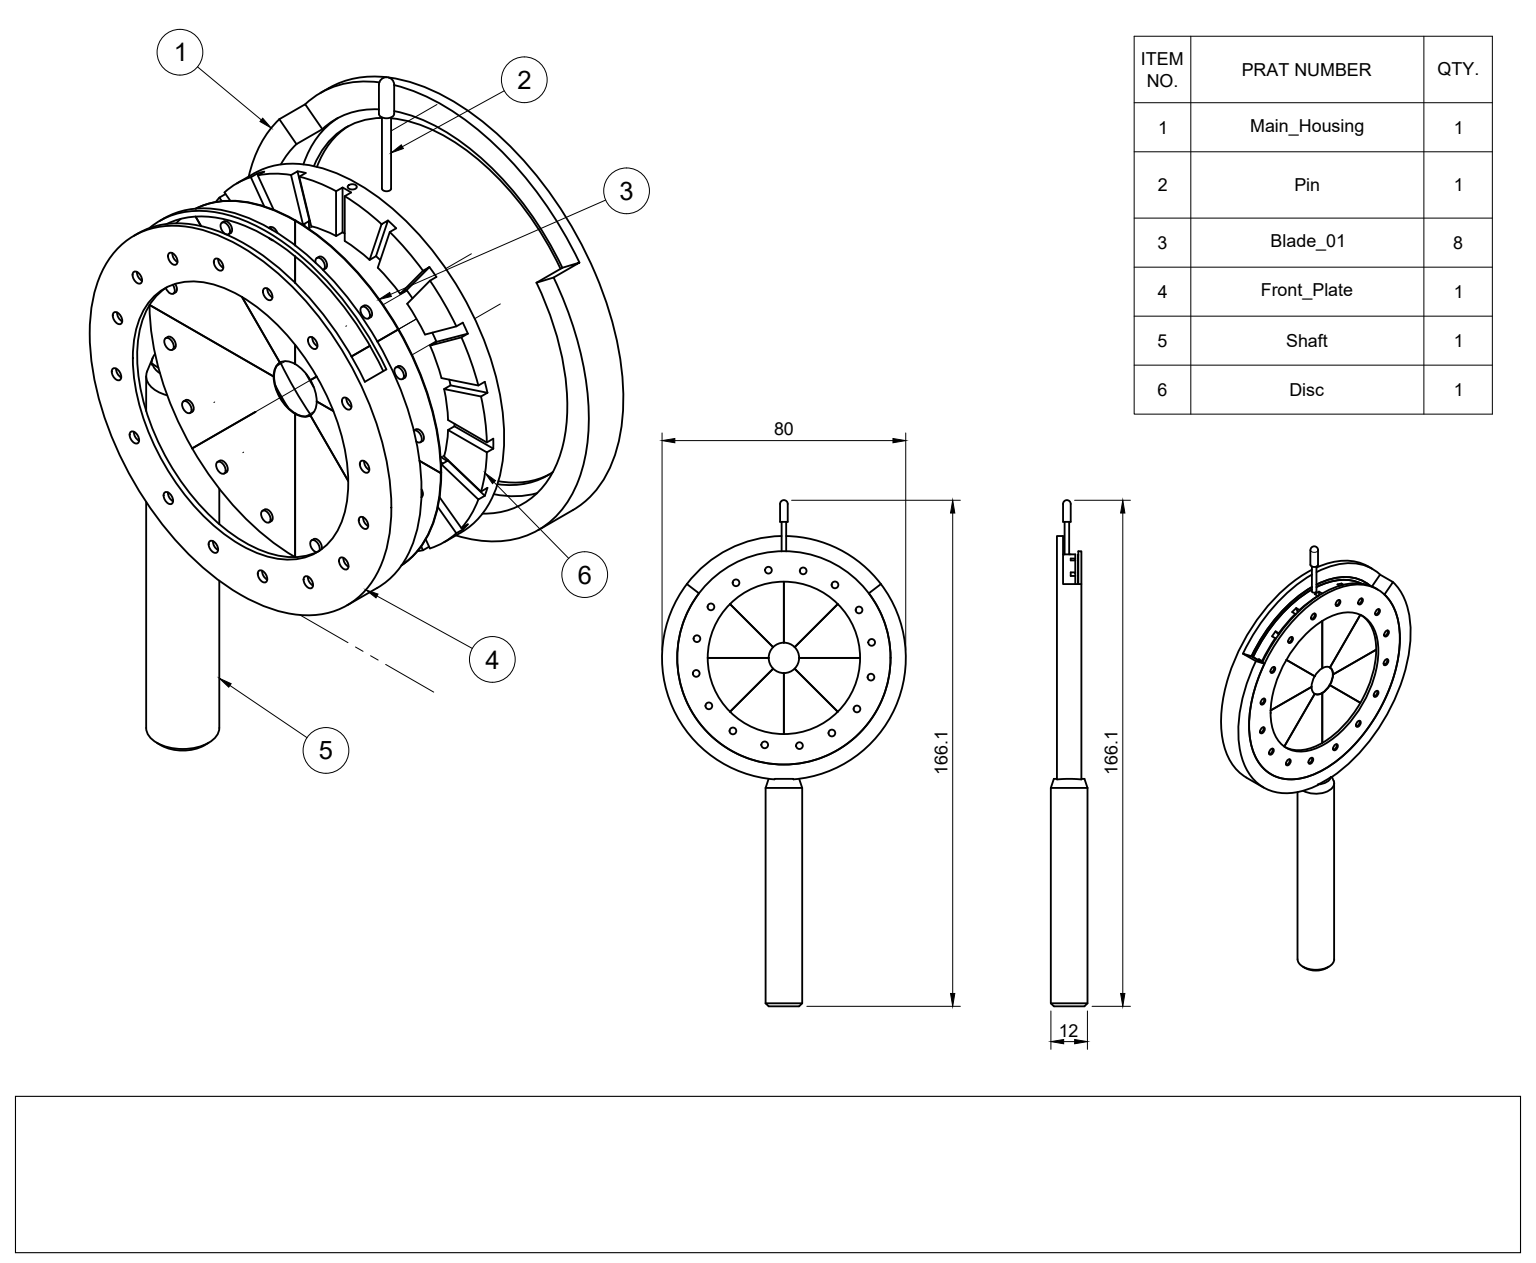
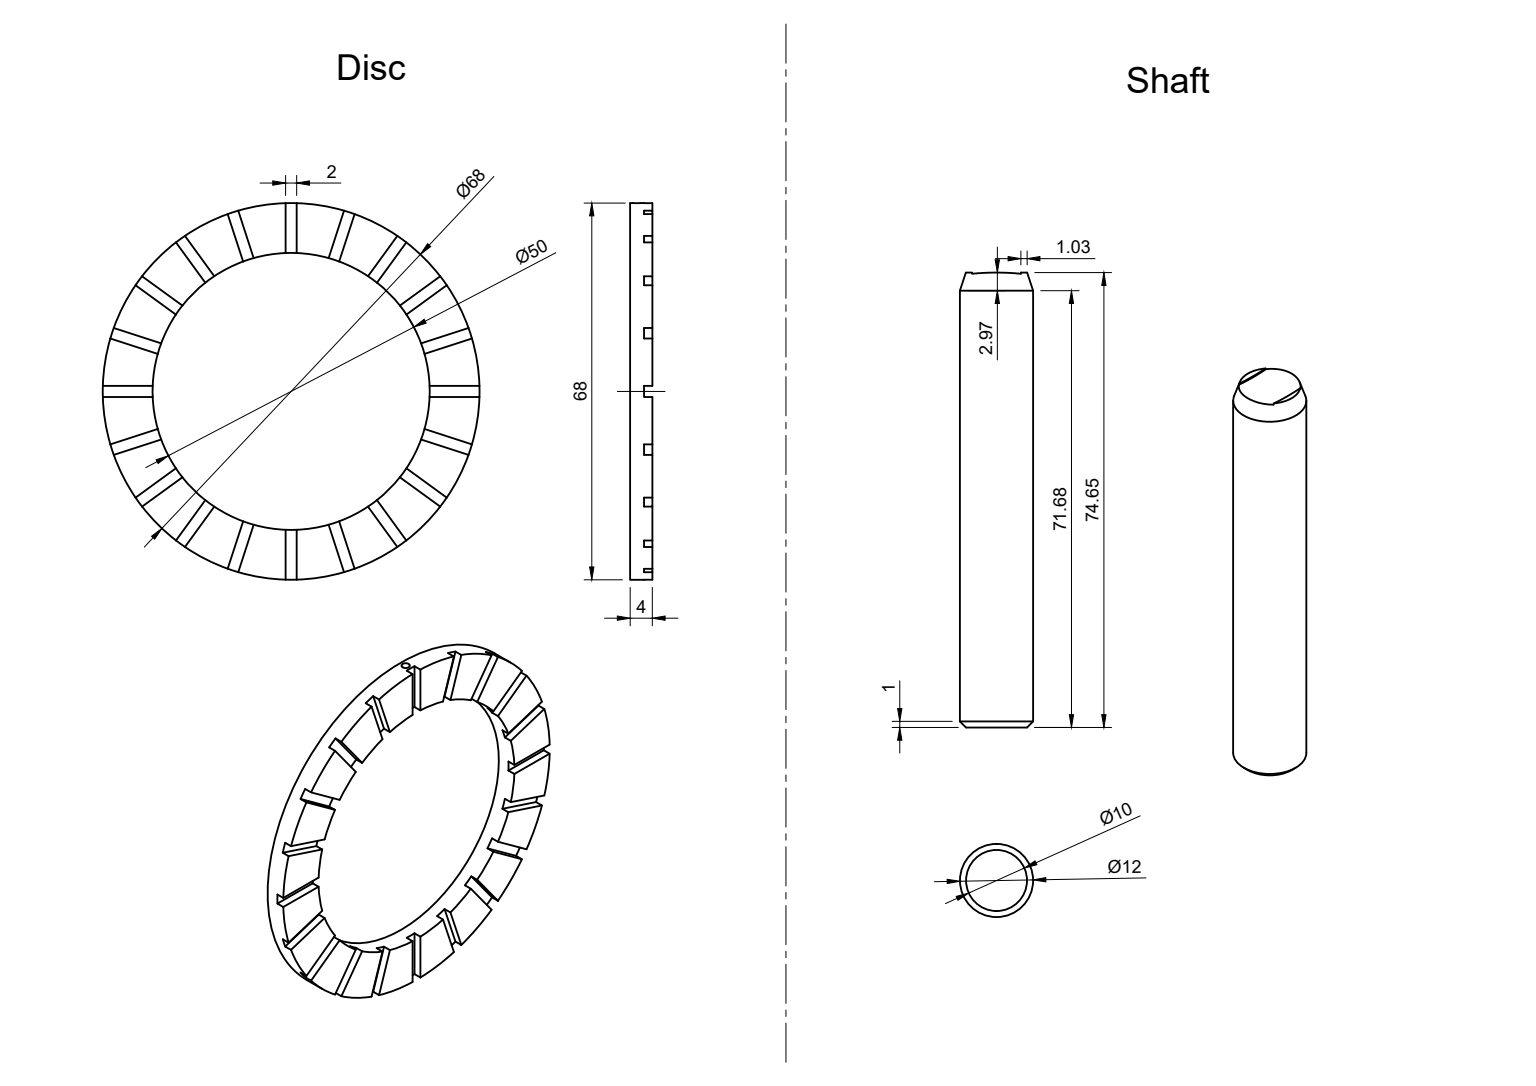
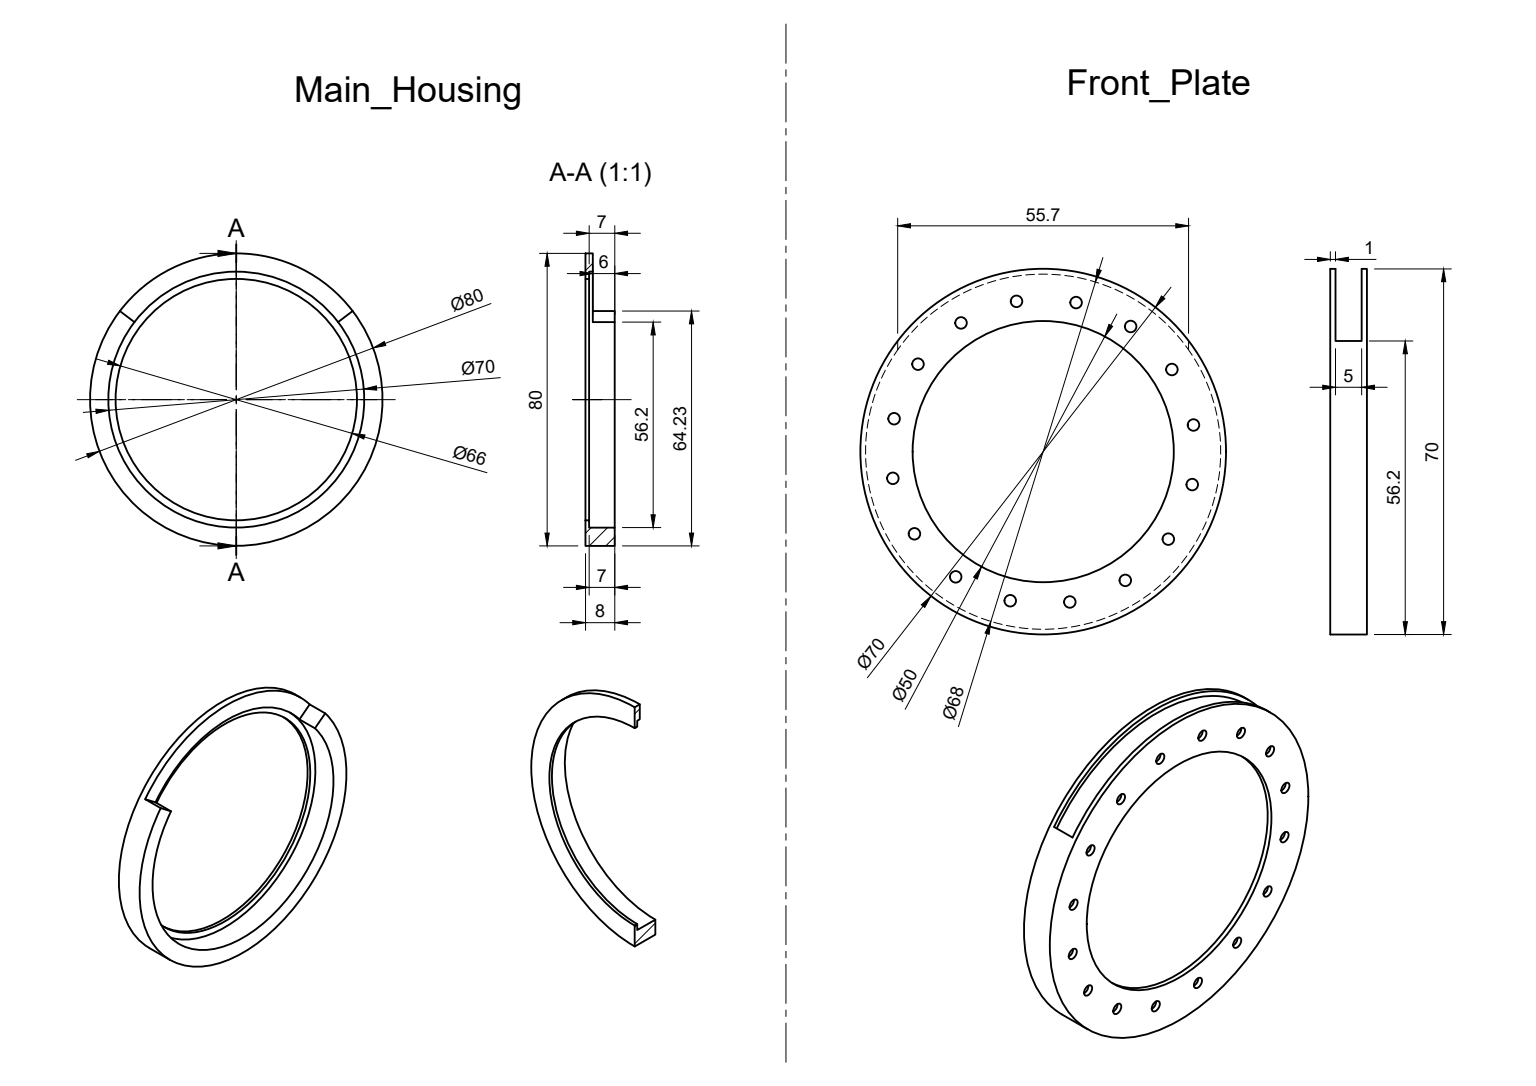
ISO-10303-21;
HEADER;
/* Generated by software containing ST-Developer
 * from STEP Tools, Inc. (www.steptools.com) 
 */

FILE_DESCRIPTION(
/* description */ (''),
/* implementation_level */ '2;1');

FILE_NAME(
/* name */ 'MAS-284',
/* time_stamp */ '2026-10-23T22:28:14+06:00',
/* author */ (''),
/* organization */ (''),
/* preprocessor_version */ 'ST-DEVELOPER v20.2',
/* originating_system */ 'Autodesk Translation Framework v15.15.0.0',
/* authorisation */ '');

FILE_SCHEMA (('AUTOMOTIVE_DESIGN { 1 0 10303 214 3 1 1 }'));
ENDSEC;

DATA;
#10=MECHANICAL_DESIGN_GEOMETRIC_PRESENTATION_REPRESENTATION('',(#103,#104,
#105,#106,#107,#108,#109,#110,#111,#112,#113,#114,#115),#6753);
#11=ITEM_DEFINED_TRANSFORMATION($,$,#3910,#4352);
#12=ITEM_DEFINED_TRANSFORMATION($,$,#3930,#4353);
#13=ITEM_DEFINED_TRANSFORMATION($,$,#3941,#4354);
#14=ITEM_DEFINED_TRANSFORMATION($,$,#3960,#4355);
#15=ITEM_DEFINED_TRANSFORMATION($,$,#4028,#4356);
#16=ITEM_DEFINED_TRANSFORMATION($,$,#4048,#4357);
#17=ITEM_DEFINED_TRANSFORMATION($,$,#4219,#4358);
#18=ITEM_DEFINED_TRANSFORMATION($,$,#4238,#4359);
#19=ITEM_DEFINED_TRANSFORMATION($,$,#4257,#4360);
#20=ITEM_DEFINED_TRANSFORMATION($,$,#4276,#4361);
#21=ITEM_DEFINED_TRANSFORMATION($,$,#4295,#4362);
#22=ITEM_DEFINED_TRANSFORMATION($,$,#4314,#4363);
#23=ITEM_DEFINED_TRANSFORMATION($,$,#4333,#4364);
#24=(
REPRESENTATION_RELATIONSHIP($,$,#6800,#6799)
REPRESENTATION_RELATIONSHIP_WITH_TRANSFORMATION(#11)
SHAPE_REPRESENTATION_RELATIONSHIP()
);
#25=(
REPRESENTATION_RELATIONSHIP($,$,#6801,#6799)
REPRESENTATION_RELATIONSHIP_WITH_TRANSFORMATION(#12)
SHAPE_REPRESENTATION_RELATIONSHIP()
);
#26=(
REPRESENTATION_RELATIONSHIP($,$,#6802,#6799)
REPRESENTATION_RELATIONSHIP_WITH_TRANSFORMATION(#13)
SHAPE_REPRESENTATION_RELATIONSHIP()
);
#27=(
REPRESENTATION_RELATIONSHIP($,$,#6803,#6799)
REPRESENTATION_RELATIONSHIP_WITH_TRANSFORMATION(#14)
SHAPE_REPRESENTATION_RELATIONSHIP()
);
#28=(
REPRESENTATION_RELATIONSHIP($,$,#6804,#6799)
REPRESENTATION_RELATIONSHIP_WITH_TRANSFORMATION(#15)
SHAPE_REPRESENTATION_RELATIONSHIP()
);
#29=(
REPRESENTATION_RELATIONSHIP($,$,#6805,#6799)
REPRESENTATION_RELATIONSHIP_WITH_TRANSFORMATION(#16)
SHAPE_REPRESENTATION_RELATIONSHIP()
);
#30=(
REPRESENTATION_RELATIONSHIP($,$,#6806,#6799)
REPRESENTATION_RELATIONSHIP_WITH_TRANSFORMATION(#17)
SHAPE_REPRESENTATION_RELATIONSHIP()
);
#31=(
REPRESENTATION_RELATIONSHIP($,$,#6807,#6799)
REPRESENTATION_RELATIONSHIP_WITH_TRANSFORMATION(#18)
SHAPE_REPRESENTATION_RELATIONSHIP()
);
#32=(
REPRESENTATION_RELATIONSHIP($,$,#6808,#6799)
REPRESENTATION_RELATIONSHIP_WITH_TRANSFORMATION(#19)
SHAPE_REPRESENTATION_RELATIONSHIP()
);
#33=(
REPRESENTATION_RELATIONSHIP($,$,#6809,#6799)
REPRESENTATION_RELATIONSHIP_WITH_TRANSFORMATION(#20)
SHAPE_REPRESENTATION_RELATIONSHIP()
);
#34=(
REPRESENTATION_RELATIONSHIP($,$,#6810,#6799)
REPRESENTATION_RELATIONSHIP_WITH_TRANSFORMATION(#21)
SHAPE_REPRESENTATION_RELATIONSHIP()
);
#35=(
REPRESENTATION_RELATIONSHIP($,$,#6811,#6799)
REPRESENTATION_RELATIONSHIP_WITH_TRANSFORMATION(#22)
SHAPE_REPRESENTATION_RELATIONSHIP()
);
#36=(
REPRESENTATION_RELATIONSHIP($,$,#6812,#6799)
REPRESENTATION_RELATIONSHIP_WITH_TRANSFORMATION(#23)
SHAPE_REPRESENTATION_RELATIONSHIP()
);
#37=CONTEXT_DEPENDENT_SHAPE_REPRESENTATION(#24,#6786);
#38=CONTEXT_DEPENDENT_SHAPE_REPRESENTATION(#25,#6787);
#39=CONTEXT_DEPENDENT_SHAPE_REPRESENTATION(#26,#6788);
#40=CONTEXT_DEPENDENT_SHAPE_REPRESENTATION(#27,#6789);
#41=CONTEXT_DEPENDENT_SHAPE_REPRESENTATION(#28,#6790);
#42=CONTEXT_DEPENDENT_SHAPE_REPRESENTATION(#29,#6791);
#43=CONTEXT_DEPENDENT_SHAPE_REPRESENTATION(#30,#6792);
#44=CONTEXT_DEPENDENT_SHAPE_REPRESENTATION(#31,#6793);
#45=CONTEXT_DEPENDENT_SHAPE_REPRESENTATION(#32,#6794);
#46=CONTEXT_DEPENDENT_SHAPE_REPRESENTATION(#33,#6795);
#47=CONTEXT_DEPENDENT_SHAPE_REPRESENTATION(#34,#6796);
#48=CONTEXT_DEPENDENT_SHAPE_REPRESENTATION(#35,#6797);
#49=CONTEXT_DEPENDENT_SHAPE_REPRESENTATION(#36,#6798);
#50=NEXT_ASSEMBLY_USAGE_OCCURRENCE('Main_Housing:1','Main_Housing:1',
'Main_Housing:1',#6814,#6815,'Main_Housing:1');
#51=NEXT_ASSEMBLY_USAGE_OCCURRENCE('Pin:1','Pin:1','Pin:1',#6814,#6816,
'Pin:1');
#52=NEXT_ASSEMBLY_USAGE_OCCURRENCE('Blade_01:1','Blade_01:1',
'Blade_01:1',#6814,#6817,'Blade_01:1');
#53=NEXT_ASSEMBLY_USAGE_OCCURRENCE('Front_Plate:1','Front_Plate:1',
'Front_Plate:1',#6814,#6818,'Front_Plate:1');
#54=NEXT_ASSEMBLY_USAGE_OCCURRENCE('Shaft:1','Shaft:1','Shaft:1',#6814,
#6819,'Shaft:1');
#55=NEXT_ASSEMBLY_USAGE_OCCURRENCE('Disc:1','Disc:1','Disc:1',#6814,#6820,
'Disc:1');
#56=NEXT_ASSEMBLY_USAGE_OCCURRENCE('Blade_02:1','Blade_02:1',
'Blade_02:1',#6814,#6821,'Blade_02:1');
#57=NEXT_ASSEMBLY_USAGE_OCCURRENCE('Blade_03:1','Blade_03:1',
'Blade_03:1',#6814,#6822,'Blade_03:1');
#58=NEXT_ASSEMBLY_USAGE_OCCURRENCE('Blade_05:1','Blade_05:1',
'Blade_05:1',#6814,#6823,'Blade_05:1');
#59=NEXT_ASSEMBLY_USAGE_OCCURRENCE('Blade_06:1','Blade_06:1',
'Blade_06:1',#6814,#6824,'Blade_06:1');
#60=NEXT_ASSEMBLY_USAGE_OCCURRENCE('Blade_07:1','Blade_07:1',
'Blade_07:1',#6814,#6825,'Blade_07:1');
#61=NEXT_ASSEMBLY_USAGE_OCCURRENCE('Blade_08:1','Blade_08:1',
'Blade_08:1',#6814,#6826,'Blade_08:1');
#62=NEXT_ASSEMBLY_USAGE_OCCURRENCE('Blade_04:1','Blade_04:1',
'Blade_04:1',#6814,#6827,'Blade_04:1');
#63=CONICAL_SURFACE('',#4040,5.5,0.785398163397448);
#64=CONICAL_SURFACE('',#4047,5.51285218418961,0.317172261260326);
#65=B_SPLINE_CURVE_WITH_KNOTS('',3,(#5826,#5827,#5828,#5829,#5830,#5831,
#5832,#5833),.UNSPECIFIED.,.F.,.F.,(4,2,2,4),(0.,0.191037328674406,0.382074657348811,
0.439575437008213),.UNSPECIFIED.);
#66=B_SPLINE_CURVE_WITH_KNOTS('',3,(#5837,#5838,#5839,#5840,#5841,#5842,
#5843,#5844),.UNSPECIFIED.,.F.,.F.,(4,2,2,4),(1.09233777373606,1.14983855339546,
1.34087588206987,1.53191321074428),.UNSPECIFIED.);
#67=B_SPLINE_CURVE_WITH_KNOTS('',3,(#5845,#5846,#5847,#5848,#5849,#5850,
#5851,#5852),.UNSPECIFIED.,.F.,.F.,(4,2,2,4),(1.53191321074428,1.72295053941868,
1.91398786809309,1.97148864775249),.UNSPECIFIED.);
#68=B_SPLINE_CURVE_WITH_KNOTS('',3,(#5853,#5854,#5855,#5856,#5857,#5858,
#5859,#5860),.UNSPECIFIED.,.F.,.F.,(4,2,2,4),(-0.439575436976826,-0.382074657348811,
-0.191037328674406,0.),.UNSPECIFIED.);
#69=B_SPLINE_CURVE_WITH_KNOTS('',3,(#5893,#5894,#5895,#5896,#5897,#5898,
#5899,#5900,#5901,#5902,#5903,#5904,#5905,#5906,#5907,#5908,#5909,#5910,
#5911,#5912,#5913,#5914,#5915,#5916,#5917,#5918,#5919,#5920,#5921,#5922,
#5923,#5924,#5925,#5926),.UNSPECIFIED.,.T.,.F.,(4,2,2,2,2,2,2,2,2,2,2,2,
2,2,2,2,4),(0.,0.0282524850207717,0.0565049700415435,0.0847574548366443,
0.113009939631745,0.141262424426846,0.169514909221947,0.197767394242719,
0.22601987926349,0.254272364284262,0.282524849305034,0.310777334100135,
0.339029818895236,0.367282303690336,0.395534788485437,0.423787273506209,
0.452039758526981),.UNSPECIFIED.);
#70=(
BOUNDED_CURVE()
B_SPLINE_CURVE(2,(#5813,#5814,#5815),.UNSPECIFIED.,.F.,.F.)
B_SPLINE_CURVE_WITH_KNOTS((3,3),(0.0138131398228909,0.0359194684117599),
 .UNSPECIFIED.)
CURVE()
GEOMETRIC_REPRESENTATION_ITEM()
RATIONAL_B_SPLINE_CURVE((1.00006551876347,1.00008518697359,1.))
REPRESENTATION_ITEM('')
);
#71=(
BOUNDED_CURVE()
B_SPLINE_CURVE(2,(#5819,#5820,#5821),.UNSPECIFIED.,.F.,.F.)
B_SPLINE_CURVE_WITH_KNOTS((3,3),(0.,0.022106328588869),.UNSPECIFIED.)
CURVE()
GEOMETRIC_REPRESENTATION_ITEM()
RATIONAL_B_SPLINE_CURVE((1.,1.00008518697359,1.00006551876347))
REPRESENTATION_ITEM('')
);
#72=(
BOUNDED_CURVE()
B_SPLINE_CURVE(2,(#5863,#5864,#5865),.UNSPECIFIED.,.F.,.F.)
B_SPLINE_CURVE_WITH_KNOTS((3,3),(0.,0.022106328588869),.UNSPECIFIED.)
CURVE()
GEOMETRIC_REPRESENTATION_ITEM()
RATIONAL_B_SPLINE_CURVE((1.,1.00008518697359,1.00006551876347))
REPRESENTATION_ITEM('')
);
#73=(
BOUNDED_CURVE()
B_SPLINE_CURVE(2,(#5868,#5869,#5870),.UNSPECIFIED.,.F.,.F.)
B_SPLINE_CURVE_WITH_KNOTS((3,3),(0.0138131398228909,0.0359194684117599),
 .UNSPECIFIED.)
CURVE()
GEOMETRIC_REPRESENTATION_ITEM()
RATIONAL_B_SPLINE_CURVE((1.00006551876347,1.00008518697359,1.))
REPRESENTATION_ITEM('')
);
#74=SPHERICAL_SURFACE('',#3931,1.25);
#75=SPHERICAL_SURFACE('',#4036,40.);
#76=SPHERICAL_SURFACE('',#4038,40.);
#77=SHAPE_REPRESENTATION_RELATIONSHIP('SRR','None',#6800,#90);
#78=SHAPE_REPRESENTATION_RELATIONSHIP('SRR','None',#6801,#91);
#79=SHAPE_REPRESENTATION_RELATIONSHIP('SRR','None',#6802,#92);
#80=SHAPE_REPRESENTATION_RELATIONSHIP('SRR','None',#6803,#93);
#81=SHAPE_REPRESENTATION_RELATIONSHIP('SRR','None',#6804,#94);
#82=SHAPE_REPRESENTATION_RELATIONSHIP('SRR','None',#6805,#95);
#83=SHAPE_REPRESENTATION_RELATIONSHIP('SRR','None',#6806,#96);
#84=SHAPE_REPRESENTATION_RELATIONSHIP('SRR','None',#6807,#97);
#85=SHAPE_REPRESENTATION_RELATIONSHIP('SRR','None',#6808,#98);
#86=SHAPE_REPRESENTATION_RELATIONSHIP('SRR','None',#6809,#99);
#87=SHAPE_REPRESENTATION_RELATIONSHIP('SRR','None',#6810,#100);
#88=SHAPE_REPRESENTATION_RELATIONSHIP('SRR','None',#6811,#101);
#89=SHAPE_REPRESENTATION_RELATIONSHIP('SRR','None',#6812,#102);
#90=ADVANCED_BREP_SHAPE_REPRESENTATION('',(#116),#6740);
#91=ADVANCED_BREP_SHAPE_REPRESENTATION('',(#117),#6741);
#92=ADVANCED_BREP_SHAPE_REPRESENTATION('',(#118),#6742);
#93=ADVANCED_BREP_SHAPE_REPRESENTATION('',(#119),#6743);
#94=ADVANCED_BREP_SHAPE_REPRESENTATION('',(#120),#6744);
#95=ADVANCED_BREP_SHAPE_REPRESENTATION('',(#121),#6745);
#96=ADVANCED_BREP_SHAPE_REPRESENTATION('',(#122),#6746);
#97=ADVANCED_BREP_SHAPE_REPRESENTATION('',(#123),#6747);
#98=ADVANCED_BREP_SHAPE_REPRESENTATION('',(#124),#6748);
#99=ADVANCED_BREP_SHAPE_REPRESENTATION('',(#125),#6749);
#100=ADVANCED_BREP_SHAPE_REPRESENTATION('',(#126),#6750);
#101=ADVANCED_BREP_SHAPE_REPRESENTATION('',(#127),#6751);
#102=ADVANCED_BREP_SHAPE_REPRESENTATION('',(#128),#6752);
#103=STYLED_ITEM('',(#6900),#116);
#104=STYLED_ITEM('',(#6921),#117);
#105=STYLED_ITEM('',(#6935),#118);
#106=STYLED_ITEM('',(#6935),#119);
#107=STYLED_ITEM('',(#6921),#120);
#108=STYLED_ITEM('',(#6907),#121);
#109=STYLED_ITEM('',(#6907),#122);
#110=STYLED_ITEM('',(#6914),#123);
#111=STYLED_ITEM('',(#6935),#124);
#112=STYLED_ITEM('',(#6935),#125);
#113=STYLED_ITEM('',(#6907),#126);
#114=STYLED_ITEM('',(#6907),#127);
#115=STYLED_ITEM('',(#6914),#128);
#116=MANIFOLD_SOLID_BREP('Main_Housing',#3752);
#117=MANIFOLD_SOLID_BREP('Pin',#3753);
#118=MANIFOLD_SOLID_BREP('Blade_01',#3754);
#119=MANIFOLD_SOLID_BREP('Front_Plate',#3755);
#120=MANIFOLD_SOLID_BREP('Shaft',#3756);
#121=MANIFOLD_SOLID_BREP('Disc',#3757);
#122=MANIFOLD_SOLID_BREP('Blade_02',#3758);
#123=MANIFOLD_SOLID_BREP('Blade_03',#3759);
#124=MANIFOLD_SOLID_BREP('Blade_05',#3760);
#125=MANIFOLD_SOLID_BREP('Blade_06',#3761);
#126=MANIFOLD_SOLID_BREP('Blade_07',#3762);
#127=MANIFOLD_SOLID_BREP('Blade_08',#3763);
#128=MANIFOLD_SOLID_BREP('Blade_04',#3764);
#129=FACE_BOUND('',#548,.T.);
#130=FACE_BOUND('',#556,.T.);
#131=FACE_BOUND('',#560,.T.);
#132=FACE_BOUND('',#566,.T.);
#133=FACE_BOUND('',#567,.T.);
#134=FACE_BOUND('',#580,.T.);
#135=FACE_BOUND('',#582,.T.);
#136=FACE_BOUND('',#601,.T.);
#137=FACE_BOUND('',#602,.T.);
#138=FACE_BOUND('',#603,.T.);
#139=FACE_BOUND('',#604,.T.);
#140=FACE_BOUND('',#605,.T.);
#141=FACE_BOUND('',#606,.T.);
#142=FACE_BOUND('',#607,.T.);
#143=FACE_BOUND('',#608,.T.);
#144=FACE_BOUND('',#609,.T.);
#145=FACE_BOUND('',#610,.T.);
#146=FACE_BOUND('',#611,.T.);
#147=FACE_BOUND('',#612,.T.);
#148=FACE_BOUND('',#613,.T.);
#149=FACE_BOUND('',#614,.T.);
#150=FACE_BOUND('',#615,.T.);
#151=FACE_BOUND('',#616,.T.);
#152=FACE_BOUND('',#617,.T.);
#153=FACE_BOUND('',#619,.T.);
#154=FACE_BOUND('',#620,.T.);
#155=FACE_BOUND('',#621,.T.);
#156=FACE_BOUND('',#622,.T.);
#157=FACE_BOUND('',#623,.T.);
#158=FACE_BOUND('',#624,.T.);
#159=FACE_BOUND('',#625,.T.);
#160=FACE_BOUND('',#626,.T.);
#161=FACE_BOUND('',#627,.T.);
#162=FACE_BOUND('',#628,.T.);
#163=FACE_BOUND('',#629,.T.);
#164=FACE_BOUND('',#630,.T.);
#165=FACE_BOUND('',#631,.T.);
#166=FACE_BOUND('',#632,.T.);
#167=FACE_BOUND('',#633,.T.);
#168=FACE_BOUND('',#634,.T.);
#169=FACE_BOUND('',#635,.T.);
#170=FACE_BOUND('',#728,.T.);
#171=FACE_BOUND('',#730,.T.);
#172=FACE_BOUND('',#735,.T.);
#173=FACE_BOUND('',#736,.T.);
#174=FACE_BOUND('',#747,.T.);
#175=FACE_BOUND('',#748,.T.);
#176=FACE_BOUND('',#759,.T.);
#177=FACE_BOUND('',#760,.T.);
#178=FACE_BOUND('',#771,.T.);
#179=FACE_BOUND('',#772,.T.);
#180=FACE_BOUND('',#783,.T.);
#181=FACE_BOUND('',#784,.T.);
#182=FACE_BOUND('',#795,.T.);
#183=FACE_BOUND('',#796,.T.);
#184=FACE_BOUND('',#807,.T.);
#185=FACE_BOUND('',#808,.T.);
#186=PLANE('',#3916);
#187=PLANE('',#3918);
#188=PLANE('',#3921);
#189=PLANE('',#3922);
#190=PLANE('',#3923);
#191=PLANE('',#3929);
#192=PLANE('',#3936);
#193=PLANE('',#3940);
#194=PLANE('',#3942);
#195=PLANE('',#3943);
#196=PLANE('',#3944);
#197=PLANE('',#3951);
#198=PLANE('',#3954);
#199=PLANE('',#3959);
#200=PLANE('',#3961);
#201=PLANE('',#3964);
#202=PLANE('',#3965);
#203=PLANE('',#3974);
#204=PLANE('',#4026);
#205=PLANE('',#4027);
#206=PLANE('',#4029);
#207=PLANE('',#4034);
#208=PLANE('',#4046);
#209=PLANE('',#4051);
#210=PLANE('',#4052);
#211=PLANE('',#4053);
#212=PLANE('',#4054);
#213=PLANE('',#4055);
#214=PLANE('',#4056);
#215=PLANE('',#4057);
#216=PLANE('',#4058);
#217=PLANE('',#4059);
#218=PLANE('',#4060);
#219=PLANE('',#4061);
#220=PLANE('',#4062);
#221=PLANE('',#4063);
#222=PLANE('',#4064);
#223=PLANE('',#4065);
#224=PLANE('',#4066);
#225=PLANE('',#4067);
#226=PLANE('',#4068);
#227=PLANE('',#4069);
#228=PLANE('',#4070);
#229=PLANE('',#4071);
#230=PLANE('',#4076);
#231=PLANE('',#4079);
#232=PLANE('',#4082);
#233=PLANE('',#4085);
#234=PLANE('',#4088);
#235=PLANE('',#4091);
#236=PLANE('',#4094);
#237=PLANE('',#4097);
#238=PLANE('',#4100);
#239=PLANE('',#4103);
#240=PLANE('',#4106);
#241=PLANE('',#4109);
#242=PLANE('',#4112);
#243=PLANE('',#4115);
#244=PLANE('',#4118);
#245=PLANE('',#4121);
#246=PLANE('',#4124);
#247=PLANE('',#4127);
#248=PLANE('',#4130);
#249=PLANE('',#4131);
#250=PLANE('',#4132);
#251=PLANE('',#4133);
#252=PLANE('',#4134);
#253=PLANE('',#4135);
#254=PLANE('',#4136);
#255=PLANE('',#4137);
#256=PLANE('',#4138);
#257=PLANE('',#4139);
#258=PLANE('',#4140);
#259=PLANE('',#4141);
#260=PLANE('',#4142);
#261=PLANE('',#4143);
#262=PLANE('',#4144);
#263=PLANE('',#4145);
#264=PLANE('',#4146);
#265=PLANE('',#4147);
#266=PLANE('',#4148);
#267=PLANE('',#4172);
#268=PLANE('',#4174);
#269=PLANE('',#4176);
#270=PLANE('',#4178);
#271=PLANE('',#4180);
#272=PLANE('',#4182);
#273=PLANE('',#4184);
#274=PLANE('',#4186);
#275=PLANE('',#4188);
#276=PLANE('',#4190);
#277=PLANE('',#4192);
#278=PLANE('',#4194);
#279=PLANE('',#4196);
#280=PLANE('',#4198);
#281=PLANE('',#4200);
#282=PLANE('',#4202);
#283=PLANE('',#4204);
#284=PLANE('',#4206);
#285=PLANE('',#4208);
#286=PLANE('',#4210);
#287=PLANE('',#4211);
#288=PLANE('',#4213);
#289=PLANE('',#4217);
#290=PLANE('',#4218);
#291=PLANE('',#4220);
#292=PLANE('',#4221);
#293=PLANE('',#4222);
#294=PLANE('',#4229);
#295=PLANE('',#4232);
#296=PLANE('',#4237);
#297=PLANE('',#4239);
#298=PLANE('',#4240);
#299=PLANE('',#4241);
#300=PLANE('',#4248);
#301=PLANE('',#4251);
#302=PLANE('',#4256);
#303=PLANE('',#4258);
#304=PLANE('',#4259);
#305=PLANE('',#4260);
#306=PLANE('',#4267);
#307=PLANE('',#4270);
#308=PLANE('',#4275);
#309=PLANE('',#4277);
#310=PLANE('',#4278);
#311=PLANE('',#4279);
#312=PLANE('',#4286);
#313=PLANE('',#4289);
#314=PLANE('',#4294);
#315=PLANE('',#4296);
#316=PLANE('',#4297);
#317=PLANE('',#4298);
#318=PLANE('',#4305);
#319=PLANE('',#4308);
#320=PLANE('',#4313);
#321=PLANE('',#4315);
#322=PLANE('',#4316);
#323=PLANE('',#4317);
#324=PLANE('',#4324);
#325=PLANE('',#4327);
#326=PLANE('',#4332);
#327=PLANE('',#4334);
#328=PLANE('',#4335);
#329=PLANE('',#4336);
#330=PLANE('',#4343);
#331=PLANE('',#4346);
#332=PLANE('',#4351);
#333=FACE_OUTER_BOUND('',#546,.T.);
#334=FACE_OUTER_BOUND('',#547,.T.);
#335=FACE_OUTER_BOUND('',#549,.T.);
#336=FACE_OUTER_BOUND('',#550,.T.);
#337=FACE_OUTER_BOUND('',#551,.T.);
#338=FACE_OUTER_BOUND('',#552,.T.);
#339=FACE_OUTER_BOUND('',#553,.T.);
#340=FACE_OUTER_BOUND('',#554,.T.);
#341=FACE_OUTER_BOUND('',#555,.T.);
#342=FACE_OUTER_BOUND('',#557,.T.);
#343=FACE_OUTER_BOUND('',#558,.T.);
#344=FACE_OUTER_BOUND('',#559,.T.);
#345=FACE_OUTER_BOUND('',#561,.T.);
#346=FACE_OUTER_BOUND('',#562,.T.);
#347=FACE_OUTER_BOUND('',#563,.T.);
#348=FACE_OUTER_BOUND('',#564,.T.);
#349=FACE_OUTER_BOUND('',#565,.T.);
#350=FACE_OUTER_BOUND('',#568,.T.);
#351=FACE_OUTER_BOUND('',#569,.T.);
#352=FACE_OUTER_BOUND('',#570,.T.);
#353=FACE_OUTER_BOUND('',#571,.T.);
#354=FACE_OUTER_BOUND('',#572,.T.);
#355=FACE_OUTER_BOUND('',#573,.T.);
#356=FACE_OUTER_BOUND('',#574,.T.);
#357=FACE_OUTER_BOUND('',#575,.T.);
#358=FACE_OUTER_BOUND('',#576,.T.);
#359=FACE_OUTER_BOUND('',#577,.T.);
#360=FACE_OUTER_BOUND('',#578,.T.);
#361=FACE_OUTER_BOUND('',#579,.T.);
#362=FACE_OUTER_BOUND('',#581,.T.);
#363=FACE_OUTER_BOUND('',#583,.T.);
#364=FACE_OUTER_BOUND('',#584,.T.);
#365=FACE_OUTER_BOUND('',#585,.T.);
#366=FACE_OUTER_BOUND('',#586,.T.);
#367=FACE_OUTER_BOUND('',#587,.T.);
#368=FACE_OUTER_BOUND('',#588,.T.);
#369=FACE_OUTER_BOUND('',#589,.T.);
#370=FACE_OUTER_BOUND('',#590,.T.);
#371=FACE_OUTER_BOUND('',#591,.T.);
#372=FACE_OUTER_BOUND('',#592,.T.);
#373=FACE_OUTER_BOUND('',#593,.T.);
#374=FACE_OUTER_BOUND('',#594,.T.);
#375=FACE_OUTER_BOUND('',#595,.T.);
#376=FACE_OUTER_BOUND('',#596,.T.);
#377=FACE_OUTER_BOUND('',#597,.T.);
#378=FACE_OUTER_BOUND('',#598,.T.);
#379=FACE_OUTER_BOUND('',#599,.T.);
#380=FACE_OUTER_BOUND('',#600,.T.);
#381=FACE_OUTER_BOUND('',#618,.T.);
#382=FACE_OUTER_BOUND('',#636,.T.);
#383=FACE_OUTER_BOUND('',#637,.T.);
#384=FACE_OUTER_BOUND('',#638,.T.);
#385=FACE_OUTER_BOUND('',#639,.T.);
#386=FACE_OUTER_BOUND('',#640,.T.);
#387=FACE_OUTER_BOUND('',#641,.T.);
#388=FACE_OUTER_BOUND('',#642,.T.);
#389=FACE_OUTER_BOUND('',#643,.T.);
#390=FACE_OUTER_BOUND('',#644,.T.);
#391=FACE_OUTER_BOUND('',#645,.T.);
#392=FACE_OUTER_BOUND('',#646,.T.);
#393=FACE_OUTER_BOUND('',#647,.T.);
#394=FACE_OUTER_BOUND('',#648,.T.);
#395=FACE_OUTER_BOUND('',#649,.T.);
#396=FACE_OUTER_BOUND('',#650,.T.);
#397=FACE_OUTER_BOUND('',#651,.T.);
#398=FACE_OUTER_BOUND('',#652,.T.);
#399=FACE_OUTER_BOUND('',#653,.T.);
#400=FACE_OUTER_BOUND('',#654,.T.);
#401=FACE_OUTER_BOUND('',#655,.T.);
#402=FACE_OUTER_BOUND('',#656,.T.);
#403=FACE_OUTER_BOUND('',#657,.T.);
#404=FACE_OUTER_BOUND('',#658,.T.);
#405=FACE_OUTER_BOUND('',#659,.T.);
#406=FACE_OUTER_BOUND('',#660,.T.);
#407=FACE_OUTER_BOUND('',#661,.T.);
#408=FACE_OUTER_BOUND('',#662,.T.);
#409=FACE_OUTER_BOUND('',#663,.T.);
#410=FACE_OUTER_BOUND('',#664,.T.);
#411=FACE_OUTER_BOUND('',#665,.T.);
#412=FACE_OUTER_BOUND('',#666,.T.);
#413=FACE_OUTER_BOUND('',#667,.T.);
#414=FACE_OUTER_BOUND('',#668,.T.);
#415=FACE_OUTER_BOUND('',#669,.T.);
#416=FACE_OUTER_BOUND('',#670,.T.);
#417=FACE_OUTER_BOUND('',#671,.T.);
#418=FACE_OUTER_BOUND('',#672,.T.);
#419=FACE_OUTER_BOUND('',#673,.T.);
#420=FACE_OUTER_BOUND('',#674,.T.);
#421=FACE_OUTER_BOUND('',#675,.T.);
#422=FACE_OUTER_BOUND('',#676,.T.);
#423=FACE_OUTER_BOUND('',#677,.T.);
#424=FACE_OUTER_BOUND('',#678,.T.);
#425=FACE_OUTER_BOUND('',#679,.T.);
#426=FACE_OUTER_BOUND('',#680,.T.);
#427=FACE_OUTER_BOUND('',#681,.T.);
#428=FACE_OUTER_BOUND('',#682,.T.);
#429=FACE_OUTER_BOUND('',#683,.T.);
#430=FACE_OUTER_BOUND('',#684,.T.);
#431=FACE_OUTER_BOUND('',#685,.T.);
#432=FACE_OUTER_BOUND('',#686,.T.);
#433=FACE_OUTER_BOUND('',#687,.T.);
#434=FACE_OUTER_BOUND('',#688,.T.);
#435=FACE_OUTER_BOUND('',#689,.T.);
#436=FACE_OUTER_BOUND('',#690,.T.);
#437=FACE_OUTER_BOUND('',#691,.T.);
#438=FACE_OUTER_BOUND('',#692,.T.);
#439=FACE_OUTER_BOUND('',#693,.T.);
#440=FACE_OUTER_BOUND('',#694,.T.);
#441=FACE_OUTER_BOUND('',#695,.T.);
#442=FACE_OUTER_BOUND('',#696,.T.);
#443=FACE_OUTER_BOUND('',#697,.T.);
#444=FACE_OUTER_BOUND('',#698,.T.);
#445=FACE_OUTER_BOUND('',#699,.T.);
#446=FACE_OUTER_BOUND('',#700,.T.);
#447=FACE_OUTER_BOUND('',#701,.T.);
#448=FACE_OUTER_BOUND('',#702,.T.);
#449=FACE_OUTER_BOUND('',#703,.T.);
#450=FACE_OUTER_BOUND('',#704,.T.);
#451=FACE_OUTER_BOUND('',#705,.T.);
#452=FACE_OUTER_BOUND('',#706,.T.);
#453=FACE_OUTER_BOUND('',#707,.T.);
#454=FACE_OUTER_BOUND('',#708,.T.);
#455=FACE_OUTER_BOUND('',#709,.T.);
#456=FACE_OUTER_BOUND('',#710,.T.);
#457=FACE_OUTER_BOUND('',#711,.T.);
#458=FACE_OUTER_BOUND('',#712,.T.);
#459=FACE_OUTER_BOUND('',#713,.T.);
#460=FACE_OUTER_BOUND('',#714,.T.);
#461=FACE_OUTER_BOUND('',#715,.T.);
#462=FACE_OUTER_BOUND('',#716,.T.);
#463=FACE_OUTER_BOUND('',#717,.T.);
#464=FACE_OUTER_BOUND('',#718,.T.);
#465=FACE_OUTER_BOUND('',#719,.T.);
#466=FACE_OUTER_BOUND('',#720,.T.);
#467=FACE_OUTER_BOUND('',#721,.T.);
#468=FACE_OUTER_BOUND('',#722,.T.);
#469=FACE_OUTER_BOUND('',#723,.T.);
#470=FACE_OUTER_BOUND('',#724,.T.);
#471=FACE_OUTER_BOUND('',#725,.T.);
#472=FACE_OUTER_BOUND('',#726,.T.);
#473=FACE_OUTER_BOUND('',#727,.T.);
#474=FACE_OUTER_BOUND('',#729,.T.);
#475=FACE_OUTER_BOUND('',#731,.T.);
#476=FACE_OUTER_BOUND('',#732,.T.);
#477=FACE_OUTER_BOUND('',#733,.T.);
#478=FACE_OUTER_BOUND('',#734,.T.);
#479=FACE_OUTER_BOUND('',#737,.T.);
#480=FACE_OUTER_BOUND('',#738,.T.);
#481=FACE_OUTER_BOUND('',#739,.T.);
#482=FACE_OUTER_BOUND('',#740,.T.);
#483=FACE_OUTER_BOUND('',#741,.T.);
#484=FACE_OUTER_BOUND('',#742,.T.);
#485=FACE_OUTER_BOUND('',#743,.T.);
#486=FACE_OUTER_BOUND('',#744,.T.);
#487=FACE_OUTER_BOUND('',#745,.T.);
#488=FACE_OUTER_BOUND('',#746,.T.);
#489=FACE_OUTER_BOUND('',#749,.T.);
#490=FACE_OUTER_BOUND('',#750,.T.);
#491=FACE_OUTER_BOUND('',#751,.T.);
#492=FACE_OUTER_BOUND('',#752,.T.);
#493=FACE_OUTER_BOUND('',#753,.T.);
#494=FACE_OUTER_BOUND('',#754,.T.);
#495=FACE_OUTER_BOUND('',#755,.T.);
#496=FACE_OUTER_BOUND('',#756,.T.);
#497=FACE_OUTER_BOUND('',#757,.T.);
#498=FACE_OUTER_BOUND('',#758,.T.);
#499=FACE_OUTER_BOUND('',#761,.T.);
#500=FACE_OUTER_BOUND('',#762,.T.);
#501=FACE_OUTER_BOUND('',#763,.T.);
#502=FACE_OUTER_BOUND('',#764,.T.);
#503=FACE_OUTER_BOUND('',#765,.T.);
#504=FACE_OUTER_BOUND('',#766,.T.);
#505=FACE_OUTER_BOUND('',#767,.T.);
#506=FACE_OUTER_BOUND('',#768,.T.);
#507=FACE_OUTER_BOUND('',#769,.T.);
#508=FACE_OUTER_BOUND('',#770,.T.);
#509=FACE_OUTER_BOUND('',#773,.T.);
#510=FACE_OUTER_BOUND('',#774,.T.);
#511=FACE_OUTER_BOUND('',#775,.T.);
#512=FACE_OUTER_BOUND('',#776,.T.);
#513=FACE_OUTER_BOUND('',#777,.T.);
#514=FACE_OUTER_BOUND('',#778,.T.);
#515=FACE_OUTER_BOUND('',#779,.T.);
#516=FACE_OUTER_BOUND('',#780,.T.);
#517=FACE_OUTER_BOUND('',#781,.T.);
#518=FACE_OUTER_BOUND('',#782,.T.);
#519=FACE_OUTER_BOUND('',#785,.T.);
#520=FACE_OUTER_BOUND('',#786,.T.);
#521=FACE_OUTER_BOUND('',#787,.T.);
#522=FACE_OUTER_BOUND('',#788,.T.);
#523=FACE_OUTER_BOUND('',#789,.T.);
#524=FACE_OUTER_BOUND('',#790,.T.);
#525=FACE_OUTER_BOUND('',#791,.T.);
#526=FACE_OUTER_BOUND('',#792,.T.);
#527=FACE_OUTER_BOUND('',#793,.T.);
#528=FACE_OUTER_BOUND('',#794,.T.);
#529=FACE_OUTER_BOUND('',#797,.T.);
#530=FACE_OUTER_BOUND('',#798,.T.);
#531=FACE_OUTER_BOUND('',#799,.T.);
#532=FACE_OUTER_BOUND('',#800,.T.);
#533=FACE_OUTER_BOUND('',#801,.T.);
#534=FACE_OUTER_BOUND('',#802,.T.);
#535=FACE_OUTER_BOUND('',#803,.T.);
#536=FACE_OUTER_BOUND('',#804,.T.);
#537=FACE_OUTER_BOUND('',#805,.T.);
#538=FACE_OUTER_BOUND('',#806,.T.);
#539=FACE_OUTER_BOUND('',#809,.T.);
#540=FACE_OUTER_BOUND('',#810,.T.);
#541=FACE_OUTER_BOUND('',#811,.T.);
#542=FACE_OUTER_BOUND('',#812,.T.);
#543=FACE_OUTER_BOUND('',#813,.T.);
#544=FACE_OUTER_BOUND('',#814,.T.);
#545=FACE_OUTER_BOUND('',#815,.T.);
#546=EDGE_LOOP('',(#2456,#2457,#2458,#2459,#2460,#2461,#2462,#2463));
#547=EDGE_LOOP('',(#2464));
#548=EDGE_LOOP('',(#2465));
#549=EDGE_LOOP('',(#2466,#2467,#2468,#2469,#2470,#2471));
#550=EDGE_LOOP('',(#2472,#2473,#2474,#2475));
#551=EDGE_LOOP('',(#2476,#2477,#2478,#2479));
#552=EDGE_LOOP('',(#2480,#2481,#2482,#2483));
#553=EDGE_LOOP('',(#2484,#2485,#2486,#2487));
#554=EDGE_LOOP('',(#2488,#2489,#2490,#2491,#2492,#2493,#2494,#2495));
#555=EDGE_LOOP('',(#2496));
#556=EDGE_LOOP('',(#2497));
#557=EDGE_LOOP('',(#2498,#2499,#2500));
#558=EDGE_LOOP('',(#2501,#2502,#2503,#2504));
#559=EDGE_LOOP('',(#2505));
#560=EDGE_LOOP('',(#2506));
#561=EDGE_LOOP('',(#2507,#2508,#2509,#2510));
#562=EDGE_LOOP('',(#2511));
#563=EDGE_LOOP('',(#2512,#2513,#2514,#2515));
#564=EDGE_LOOP('',(#2516,#2517,#2518,#2519));
#565=EDGE_LOOP('',(#2520,#2521,#2522,#2523));
#566=EDGE_LOOP('',(#2524));
#567=EDGE_LOOP('',(#2525));
#568=EDGE_LOOP('',(#2526,#2527,#2528,#2529));
#569=EDGE_LOOP('',(#2530));
#570=EDGE_LOOP('',(#2531,#2532,#2533,#2534));
#571=EDGE_LOOP('',(#2535));
#572=EDGE_LOOP('',(#2536,#2537,#2538,#2539));
#573=EDGE_LOOP('',(#2540,#2541,#2542,#2543));
#574=EDGE_LOOP('',(#2544,#2545,#2546,#2547));
#575=EDGE_LOOP('',(#2548,#2549,#2550,#2551));
#576=EDGE_LOOP('',(#2552,#2553,#2554,#2555));
#577=EDGE_LOOP('',(#2556,#2557,#2558,#2559));
#578=EDGE_LOOP('',(#2560,#2561,#2562,#2563,#2564,#2565,#2566,#2567));
#579=EDGE_LOOP('',(#2568,#2569,#2570,#2571));
#580=EDGE_LOOP('',(#2572,#2573,#2574,#2575));
#581=EDGE_LOOP('',(#2576));
#582=EDGE_LOOP('',(#2577));
#583=EDGE_LOOP('',(#2578,#2579,#2580,#2581));
#584=EDGE_LOOP('',(#2582,#2583,#2584,#2585));
#585=EDGE_LOOP('',(#2586,#2587,#2588,#2589));
#586=EDGE_LOOP('',(#2590,#2591,#2592,#2593));
#587=EDGE_LOOP('',(#2594,#2595,#2596,#2597));
#588=EDGE_LOOP('',(#2598,#2599,#2600,#2601));
#589=EDGE_LOOP('',(#2602,#2603,#2604,#2605));
#590=EDGE_LOOP('',(#2606,#2607,#2608,#2609));
#591=EDGE_LOOP('',(#2610,#2611,#2612,#2613));
#592=EDGE_LOOP('',(#2614,#2615,#2616,#2617));
#593=EDGE_LOOP('',(#2618,#2619,#2620,#2621));
#594=EDGE_LOOP('',(#2622,#2623,#2624,#2625));
#595=EDGE_LOOP('',(#2626,#2627,#2628,#2629));
#596=EDGE_LOOP('',(#2630,#2631,#2632,#2633));
#597=EDGE_LOOP('',(#2634,#2635,#2636,#2637));
#598=EDGE_LOOP('',(#2638,#2639,#2640,#2641));
#599=EDGE_LOOP('',(#2642,#2643,#2644,#2645));
#600=EDGE_LOOP('',(#2646));
#601=EDGE_LOOP('',(#2647));
#602=EDGE_LOOP('',(#2648));
#603=EDGE_LOOP('',(#2649));
#604=EDGE_LOOP('',(#2650));
#605=EDGE_LOOP('',(#2651));
#606=EDGE_LOOP('',(#2652));
#607=EDGE_LOOP('',(#2653));
#608=EDGE_LOOP('',(#2654));
#609=EDGE_LOOP('',(#2655));
#610=EDGE_LOOP('',(#2656));
#611=EDGE_LOOP('',(#2657));
#612=EDGE_LOOP('',(#2658));
#613=EDGE_LOOP('',(#2659));
#614=EDGE_LOOP('',(#2660));
#615=EDGE_LOOP('',(#2661));
#616=EDGE_LOOP('',(#2662));
#617=EDGE_LOOP('',(#2663));
#618=EDGE_LOOP('',(#2664,#2665,#2666,#2667,#2668));
#619=EDGE_LOOP('',(#2669));
#620=EDGE_LOOP('',(#2670));
#621=EDGE_LOOP('',(#2671));
#622=EDGE_LOOP('',(#2672));
#623=EDGE_LOOP('',(#2673));
#624=EDGE_LOOP('',(#2674));
#625=EDGE_LOOP('',(#2675));
#626=EDGE_LOOP('',(#2676));
#627=EDGE_LOOP('',(#2677));
#628=EDGE_LOOP('',(#2678));
#629=EDGE_LOOP('',(#2679));
#630=EDGE_LOOP('',(#2680));
#631=EDGE_LOOP('',(#2681));
#632=EDGE_LOOP('',(#2682));
#633=EDGE_LOOP('',(#2683));
#634=EDGE_LOOP('',(#2684));
#635=EDGE_LOOP('',(#2685));
#636=EDGE_LOOP('',(#2686,#2687,#2688,#2689));
#637=EDGE_LOOP('',(#2690,#2691,#2692,#2693,#2694,#2695));
#638=EDGE_LOOP('',(#2696,#2697,#2698,#2699));
#639=EDGE_LOOP('',(#2700,#2701));
#640=EDGE_LOOP('',(#2702,#2703));
#641=EDGE_LOOP('',(#2704,#2705,#2706,#2707,#2708));
#642=EDGE_LOOP('',(#2709,#2710,#2711,#2712,#2713));
#643=EDGE_LOOP('',(#2714));
#644=EDGE_LOOP('',(#2715,#2716,#2717,#2718,#2719,#2720,#2721,#2722,#2723,
#2724,#2725,#2726,#2727));
#645=EDGE_LOOP('',(#2728,#2729,#2730,#2731));
#646=EDGE_LOOP('',(#2732));
#647=EDGE_LOOP('',(#2733,#2734,#2735,#2736));
#648=EDGE_LOOP('',(#2737,#2738,#2739,#2740));
#649=EDGE_LOOP('',(#2741,#2742,#2743,#2744));
#650=EDGE_LOOP('',(#2745,#2746,#2747,#2748));
#651=EDGE_LOOP('',(#2749,#2750,#2751,#2752));
#652=EDGE_LOOP('',(#2753,#2754,#2755,#2756));
#653=EDGE_LOOP('',(#2757,#2758,#2759,#2760));
#654=EDGE_LOOP('',(#2761,#2762,#2763,#2764));
#655=EDGE_LOOP('',(#2765,#2766,#2767,#2768));
#656=EDGE_LOOP('',(#2769,#2770,#2771,#2772));
#657=EDGE_LOOP('',(#2773,#2774,#2775,#2776));
#658=EDGE_LOOP('',(#2777,#2778,#2779,#2780));
#659=EDGE_LOOP('',(#2781,#2782,#2783,#2784));
#660=EDGE_LOOP('',(#2785,#2786,#2787,#2788));
#661=EDGE_LOOP('',(#2789,#2790,#2791,#2792));
#662=EDGE_LOOP('',(#2793,#2794,#2795,#2796));
#663=EDGE_LOOP('',(#2797,#2798,#2799,#2800));
#664=EDGE_LOOP('',(#2801,#2802,#2803,#2804));
#665=EDGE_LOOP('',(#2805,#2806,#2807,#2808));
#666=EDGE_LOOP('',(#2809,#2810,#2811,#2812,#2813,#2814));
#667=EDGE_LOOP('',(#2815,#2816,#2817,#2818));
#668=EDGE_LOOP('',(#2819,#2820,#2821,#2822));
#669=EDGE_LOOP('',(#2823,#2824,#2825,#2826));
#670=EDGE_LOOP('',(#2827,#2828,#2829,#2830));
#671=EDGE_LOOP('',(#2831,#2832,#2833,#2834));
#672=EDGE_LOOP('',(#2835,#2836,#2837,#2838));
#673=EDGE_LOOP('',(#2839,#2840,#2841,#2842));
#674=EDGE_LOOP('',(#2843,#2844,#2845,#2846));
#675=EDGE_LOOP('',(#2847,#2848,#2849,#2850));
#676=EDGE_LOOP('',(#2851,#2852,#2853,#2854));
#677=EDGE_LOOP('',(#2855,#2856,#2857,#2858));
#678=EDGE_LOOP('',(#2859,#2860,#2861,#2862));
#679=EDGE_LOOP('',(#2863,#2864,#2865,#2866));
#680=EDGE_LOOP('',(#2867,#2868,#2869,#2870));
#681=EDGE_LOOP('',(#2871,#2872,#2873,#2874));
#682=EDGE_LOOP('',(#2875,#2876,#2877,#2878));
#683=EDGE_LOOP('',(#2879,#2880,#2881,#2882));
#684=EDGE_LOOP('',(#2883,#2884,#2885,#2886));
#685=EDGE_LOOP('',(#2887,#2888,#2889,#2890));
#686=EDGE_LOOP('',(#2891,#2892,#2893,#2894));
#687=EDGE_LOOP('',(#2895,#2896,#2897,#2898));
#688=EDGE_LOOP('',(#2899,#2900,#2901,#2902));
#689=EDGE_LOOP('',(#2903,#2904,#2905,#2906));
#690=EDGE_LOOP('',(#2907,#2908,#2909,#2910));
#691=EDGE_LOOP('',(#2911,#2912,#2913,#2914));
#692=EDGE_LOOP('',(#2915,#2916,#2917,#2918));
#693=EDGE_LOOP('',(#2919,#2920,#2921,#2922));
#694=EDGE_LOOP('',(#2923,#2924,#2925,#2926));
#695=EDGE_LOOP('',(#2927,#2928,#2929,#2930));
#696=EDGE_LOOP('',(#2931,#2932,#2933,#2934));
#697=EDGE_LOOP('',(#2935,#2936,#2937,#2938));
#698=EDGE_LOOP('',(#2939,#2940,#2941,#2942));
#699=EDGE_LOOP('',(#2943,#2944,#2945,#2946));
#700=EDGE_LOOP('',(#2947,#2948,#2949,#2950));
#701=EDGE_LOOP('',(#2951,#2952,#2953,#2954));
#702=EDGE_LOOP('',(#2955,#2956,#2957,#2958));
#703=EDGE_LOOP('',(#2959,#2960,#2961,#2962));
#704=EDGE_LOOP('',(#2963,#2964,#2965,#2966,#2967,#2968,#2969,#2970,#2971,
#2972,#2973,#2974,#2975,#2976,#2977,#2978,#2979,#2980,#2981,#2982,#2983,
#2984,#2985,#2986,#2987,#2988,#2989,#2990,#2991,#2992,#2993,#2994,#2995,
#2996,#2997,#2998,#2999,#3000,#3001,#3002,#3003,#3004,#3005,#3006,#3007,
#3008,#3009,#3010,#3011,#3012,#3013,#3014,#3015,#3016,#3017,#3018,#3019,
#3020,#3021,#3022,#3023,#3024,#3025,#3026,#3027,#3028,#3029,#3030,#3031,
#3032,#3033,#3034,#3035,#3036,#3037,#3038,#3039,#3040,#3041,#3042,#3043,
#3044,#3045,#3046));
#705=EDGE_LOOP('',(#3047,#3048,#3049,#3050));
#706=EDGE_LOOP('',(#3051,#3052,#3053,#3054));
#707=EDGE_LOOP('',(#3055,#3056,#3057,#3058));
#708=EDGE_LOOP('',(#3059,#3060,#3061,#3062));
#709=EDGE_LOOP('',(#3063,#3064,#3065,#3066));
#710=EDGE_LOOP('',(#3067,#3068,#3069,#3070));
#711=EDGE_LOOP('',(#3071,#3072,#3073,#3074));
#712=EDGE_LOOP('',(#3075,#3076,#3077,#3078));
#713=EDGE_LOOP('',(#3079,#3080,#3081,#3082));
#714=EDGE_LOOP('',(#3083,#3084,#3085,#3086));
#715=EDGE_LOOP('',(#3087,#3088,#3089,#3090));
#716=EDGE_LOOP('',(#3091,#3092,#3093,#3094));
#717=EDGE_LOOP('',(#3095,#3096,#3097,#3098));
#718=EDGE_LOOP('',(#3099,#3100,#3101,#3102));
#719=EDGE_LOOP('',(#3103,#3104,#3105,#3106));
#720=EDGE_LOOP('',(#3107,#3108,#3109,#3110));
#721=EDGE_LOOP('',(#3111,#3112,#3113,#3114));
#722=EDGE_LOOP('',(#3115,#3116,#3117,#3118));
#723=EDGE_LOOP('',(#3119,#3120,#3121,#3122));
#724=EDGE_LOOP('',(#3123,#3124,#3125,#3126));
#725=EDGE_LOOP('',(#3127,#3128,#3129,#3130));
#726=EDGE_LOOP('',(#3131,#3132,#3133,#3134));
#727=EDGE_LOOP('',(#3135,#3136,#3137,#3138,#3139,#3140,#3141,#3142,#3143,
#3144,#3145,#3146,#3147,#3148,#3149,#3150,#3151,#3152,#3153,#3154,#3155,
#3156,#3157,#3158,#3159,#3160,#3161,#3162,#3163,#3164,#3165,#3166,#3167,
#3168,#3169,#3170,#3171,#3172,#3173,#3174,#3175,#3176,#3177,#3178,#3179,
#3180,#3181,#3182,#3183,#3184,#3185,#3186,#3187,#3188,#3189,#3190,#3191,
#3192,#3193,#3194,#3195,#3196,#3197,#3198,#3199,#3200,#3201,#3202,#3203,
#3204,#3205,#3206,#3207,#3208,#3209,#3210,#3211,#3212,#3213,#3214,#3215,
#3216,#3217,#3218));
#728=EDGE_LOOP('',(#3219));
#729=EDGE_LOOP('',(#3220));
#730=EDGE_LOOP('',(#3221));
#731=EDGE_LOOP('',(#3222,#3223,#3224,#3225));
#732=EDGE_LOOP('',(#3226,#3227,#3228,#3229));
#733=EDGE_LOOP('',(#3230,#3231,#3232,#3233));
#734=EDGE_LOOP('',(#3234,#3235,#3236,#3237));
#735=EDGE_LOOP('',(#3238));
#736=EDGE_LOOP('',(#3239));
#737=EDGE_LOOP('',(#3240,#3241,#3242,#3243));
#738=EDGE_LOOP('',(#3244));
#739=EDGE_LOOP('',(#3245,#3246,#3247,#3248));
#740=EDGE_LOOP('',(#3249));
#741=EDGE_LOOP('',(#3250,#3251,#3252,#3253));
#742=EDGE_LOOP('',(#3254,#3255,#3256,#3257));
#743=EDGE_LOOP('',(#3258,#3259,#3260,#3261));
#744=EDGE_LOOP('',(#3262,#3263,#3264,#3265));
#745=EDGE_LOOP('',(#3266,#3267,#3268,#3269));
#746=EDGE_LOOP('',(#3270,#3271,#3272,#3273));
#747=EDGE_LOOP('',(#3274));
#748=EDGE_LOOP('',(#3275));
#749=EDGE_LOOP('',(#3276,#3277,#3278,#3279));
#750=EDGE_LOOP('',(#3280));
#751=EDGE_LOOP('',(#3281,#3282,#3283,#3284));
#752=EDGE_LOOP('',(#3285));
#753=EDGE_LOOP('',(#3286,#3287,#3288,#3289));
#754=EDGE_LOOP('',(#3290,#3291,#3292,#3293));
#755=EDGE_LOOP('',(#3294,#3295,#3296,#3297));
#756=EDGE_LOOP('',(#3298,#3299,#3300,#3301));
#757=EDGE_LOOP('',(#3302,#3303,#3304,#3305));
#758=EDGE_LOOP('',(#3306,#3307,#3308,#3309));
#759=EDGE_LOOP('',(#3310));
#760=EDGE_LOOP('',(#3311));
#761=EDGE_LOOP('',(#3312,#3313,#3314,#3315));
#762=EDGE_LOOP('',(#3316));
#763=EDGE_LOOP('',(#3317,#3318,#3319,#3320));
#764=EDGE_LOOP('',(#3321));
#765=EDGE_LOOP('',(#3322,#3323,#3324,#3325));
#766=EDGE_LOOP('',(#3326,#3327,#3328,#3329));
#767=EDGE_LOOP('',(#3330,#3331,#3332,#3333));
#768=EDGE_LOOP('',(#3334,#3335,#3336,#3337));
#769=EDGE_LOOP('',(#3338,#3339,#3340,#3341));
#770=EDGE_LOOP('',(#3342,#3343,#3344,#3345));
#771=EDGE_LOOP('',(#3346));
#772=EDGE_LOOP('',(#3347));
#773=EDGE_LOOP('',(#3348,#3349,#3350,#3351));
#774=EDGE_LOOP('',(#3352));
#775=EDGE_LOOP('',(#3353,#3354,#3355,#3356));
#776=EDGE_LOOP('',(#3357));
#777=EDGE_LOOP('',(#3358,#3359,#3360,#3361));
#778=EDGE_LOOP('',(#3362,#3363,#3364,#3365));
#779=EDGE_LOOP('',(#3366,#3367,#3368,#3369));
#780=EDGE_LOOP('',(#3370,#3371,#3372,#3373));
#781=EDGE_LOOP('',(#3374,#3375,#3376,#3377));
#782=EDGE_LOOP('',(#3378,#3379,#3380,#3381));
#783=EDGE_LOOP('',(#3382));
#784=EDGE_LOOP('',(#3383));
#785=EDGE_LOOP('',(#3384,#3385,#3386,#3387));
#786=EDGE_LOOP('',(#3388));
#787=EDGE_LOOP('',(#3389,#3390,#3391,#3392));
#788=EDGE_LOOP('',(#3393));
#789=EDGE_LOOP('',(#3394,#3395,#3396,#3397));
#790=EDGE_LOOP('',(#3398,#3399,#3400,#3401));
#791=EDGE_LOOP('',(#3402,#3403,#3404,#3405));
#792=EDGE_LOOP('',(#3406,#3407,#3408,#3409));
#793=EDGE_LOOP('',(#3410,#3411,#3412,#3413));
#794=EDGE_LOOP('',(#3414,#3415,#3416,#3417));
#795=EDGE_LOOP('',(#3418));
#796=EDGE_LOOP('',(#3419));
#797=EDGE_LOOP('',(#3420,#3421,#3422,#3423));
#798=EDGE_LOOP('',(#3424));
#799=EDGE_LOOP('',(#3425,#3426,#3427,#3428));
#800=EDGE_LOOP('',(#3429));
#801=EDGE_LOOP('',(#3430,#3431,#3432,#3433));
#802=EDGE_LOOP('',(#3434,#3435,#3436,#3437));
#803=EDGE_LOOP('',(#3438,#3439,#3440,#3441));
#804=EDGE_LOOP('',(#3442,#3443,#3444,#3445));
#805=EDGE_LOOP('',(#3446,#3447,#3448,#3449));
#806=EDGE_LOOP('',(#3450,#3451,#3452,#3453));
#807=EDGE_LOOP('',(#3454));
#808=EDGE_LOOP('',(#3455));
#809=EDGE_LOOP('',(#3456,#3457,#3458,#3459));
#810=EDGE_LOOP('',(#3460));
#811=EDGE_LOOP('',(#3461,#3462,#3463,#3464));
#812=EDGE_LOOP('',(#3465));
#813=EDGE_LOOP('',(#3466,#3467,#3468,#3469));
#814=EDGE_LOOP('',(#3470,#3471,#3472,#3473));
#815=EDGE_LOOP('',(#3474,#3475,#3476,#3477));
#816=CIRCLE('',#3912,35.);
#817=CIRCLE('',#3913,35.);
#818=CIRCLE('',#3914,35.);
#819=CIRCLE('',#3915,35.);
#820=CIRCLE('',#3917,33.);
#821=CIRCLE('',#3919,40.);
#822=CIRCLE('',#3920,40.);
#823=CIRCLE('',#3924,40.);
#824=CIRCLE('',#3926,33.);
#825=CIRCLE('',#3928,40.);
#826=CIRCLE('',#3932,1.25);
#827=CIRCLE('',#3933,1.25);
#828=CIRCLE('',#3935,1.25);
#829=CIRCLE('',#3937,0.75);
#830=CIRCLE('',#3939,0.75);
#831=CIRCLE('',#3945,33.8);
#832=CIRCLE('',#3946,4.99999999999999);
#833=CIRCLE('',#3947,1.1);
#834=CIRCLE('',#3948,1.1);
#835=CIRCLE('',#3950,1.1);
#836=CIRCLE('',#3953,1.1);
#837=CIRCLE('',#3956,4.99999999999999);
#838=CIRCLE('',#3958,33.8);
#839=CIRCLE('',#3962,34.);
#840=CIRCLE('',#3963,35.);
#841=CIRCLE('',#3967,34.);
#842=CIRCLE('',#3968,34.);
#843=CIRCLE('',#3969,34.);
#844=CIRCLE('',#3971,35.);
#845=CIRCLE('',#3972,35.);
#846=CIRCLE('',#3973,35.);
#847=CIRCLE('',#3976,1.1);
#848=CIRCLE('',#3977,1.1);
#849=CIRCLE('',#3979,1.1);
#850=CIRCLE('',#3980,1.1);
#851=CIRCLE('',#3982,25.);
#852=CIRCLE('',#3983,25.);
#853=CIRCLE('',#3985,1.1);
#854=CIRCLE('',#3986,1.1);
#855=CIRCLE('',#3988,1.1);
#856=CIRCLE('',#3989,1.1);
#857=CIRCLE('',#3991,1.1);
#858=CIRCLE('',#3992,1.1);
#859=CIRCLE('',#3994,1.1);
#860=CIRCLE('',#3995,1.1);
#861=CIRCLE('',#3997,1.1);
#862=CIRCLE('',#3998,1.1);
#863=CIRCLE('',#4000,1.1);
#864=CIRCLE('',#4001,1.1);
#865=CIRCLE('',#4003,1.1);
#866=CIRCLE('',#4004,1.1);
#867=CIRCLE('',#4006,1.1);
#868=CIRCLE('',#4007,1.1);
#869=CIRCLE('',#4009,1.1);
#870=CIRCLE('',#4010,1.1);
#871=CIRCLE('',#4012,1.1);
#872=CIRCLE('',#4013,1.1);
#873=CIRCLE('',#4015,1.1);
#874=CIRCLE('',#4016,1.1);
#875=CIRCLE('',#4018,1.1);
#876=CIRCLE('',#4019,1.1);
#877=CIRCLE('',#4021,1.1);
#878=CIRCLE('',#4022,1.1);
#879=CIRCLE('',#4024,1.1);
#880=CIRCLE('',#4025,1.1);
#881=CIRCLE('',#4030,40.);
#882=CIRCLE('',#4031,39.7994974842648);
#883=CIRCLE('',#4033,40.);
#884=CIRCLE('',#4035,39.7994974842648);
#885=CIRCLE('',#4037,5.02570436837922);
#886=CIRCLE('',#4039,5.02570436837922);
#887=CIRCLE('',#4041,5.);
#888=CIRCLE('',#4042,6.);
#889=CIRCLE('',#4043,6.);
#890=CIRCLE('',#4045,6.);
#891=CIRCLE('',#4050,0.75);
#892=CIRCLE('',#4072,25.);
#893=CIRCLE('',#4073,34.);
#894=CIRCLE('',#4074,34.);
#895=CIRCLE('',#4075,25.);
#896=CIRCLE('',#4077,25.);
#897=CIRCLE('',#4078,34.);
#898=CIRCLE('',#4080,25.);
#899=CIRCLE('',#4081,34.);
#900=CIRCLE('',#4083,25.);
#901=CIRCLE('',#4084,34.);
#902=CIRCLE('',#4086,25.);
#903=CIRCLE('',#4087,34.);
#904=CIRCLE('',#4089,25.);
#905=CIRCLE('',#4090,34.);
#906=CIRCLE('',#4092,25.);
#907=CIRCLE('',#4093,34.);
#908=CIRCLE('',#4095,25.);
#909=CIRCLE('',#4096,34.);
#910=CIRCLE('',#4098,25.);
#911=CIRCLE('',#4099,34.);
#912=CIRCLE('',#4101,25.);
#913=CIRCLE('',#4102,34.);
#914=CIRCLE('',#4104,25.);
#915=CIRCLE('',#4105,34.);
#916=CIRCLE('',#4107,25.);
#917=CIRCLE('',#4108,34.);
#918=CIRCLE('',#4110,25.);
#919=CIRCLE('',#4111,34.);
#920=CIRCLE('',#4113,25.);
#921=CIRCLE('',#4114,34.);
#922=CIRCLE('',#4116,25.);
#923=CIRCLE('',#4117,34.);
#924=CIRCLE('',#4119,25.);
#925=CIRCLE('',#4120,34.);
#926=CIRCLE('',#4122,25.);
#927=CIRCLE('',#4123,34.);
#928=CIRCLE('',#4125,25.);
#929=CIRCLE('',#4126,34.);
#930=CIRCLE('',#4128,25.);
#931=CIRCLE('',#4129,34.);
#932=CIRCLE('',#4150,25.);
#933=CIRCLE('',#4151,25.);
#934=CIRCLE('',#4152,25.);
#935=CIRCLE('',#4153,25.);
#936=CIRCLE('',#4154,25.);
#937=CIRCLE('',#4155,25.);
#938=CIRCLE('',#4156,25.);
#939=CIRCLE('',#4157,25.);
#940=CIRCLE('',#4158,25.);
#941=CIRCLE('',#4159,25.);
#942=CIRCLE('',#4160,25.);
#943=CIRCLE('',#4161,25.);
#944=CIRCLE('',#4162,25.);
#945=CIRCLE('',#4163,25.);
#946=CIRCLE('',#4164,25.);
#947=CIRCLE('',#4165,25.);
#948=CIRCLE('',#4166,25.);
#949=CIRCLE('',#4167,25.);
#950=CIRCLE('',#4168,25.);
#951=CIRCLE('',#4169,25.);
#952=CIRCLE('',#4170,25.);
#953=CIRCLE('',#4171,25.);
#954=CIRCLE('',#4173,34.);
#955=CIRCLE('',#4175,34.);
#956=CIRCLE('',#4177,34.);
#957=CIRCLE('',#4179,34.);
#958=CIRCLE('',#4181,34.);
#959=CIRCLE('',#4183,34.);
#960=CIRCLE('',#4185,34.);
#961=CIRCLE('',#4187,34.);
#962=CIRCLE('',#4189,34.);
#963=CIRCLE('',#4191,34.);
#964=CIRCLE('',#4193,34.);
#965=CIRCLE('',#4195,34.);
#966=CIRCLE('',#4197,34.);
#967=CIRCLE('',#4199,34.);
#968=CIRCLE('',#4201,34.);
#969=CIRCLE('',#4203,34.);
#970=CIRCLE('',#4205,34.);
#971=CIRCLE('',#4207,34.);
#972=CIRCLE('',#4209,34.);
#973=CIRCLE('',#4212,34.);
#974=CIRCLE('',#4215,34.);
#975=CIRCLE('',#4216,34.);
#976=CIRCLE('',#4223,33.8);
#977=CIRCLE('',#4224,4.99999999999999);
#978=CIRCLE('',#4225,1.1);
#979=CIRCLE('',#4226,1.1);
#980=CIRCLE('',#4228,1.1);
#981=CIRCLE('',#4231,1.1);
#982=CIRCLE('',#4234,4.99999999999999);
#983=CIRCLE('',#4236,33.8);
#984=CIRCLE('',#4242,33.8);
#985=CIRCLE('',#4243,4.99999999999999);
#986=CIRCLE('',#4244,1.1);
#987=CIRCLE('',#4245,1.1);
#988=CIRCLE('',#4247,1.1);
#989=CIRCLE('',#4250,1.1);
#990=CIRCLE('',#4253,4.99999999999999);
#991=CIRCLE('',#4255,33.8);
#992=CIRCLE('',#4261,33.8);
#993=CIRCLE('',#4262,4.99999999999999);
#994=CIRCLE('',#4263,1.1);
#995=CIRCLE('',#4264,1.1);
#996=CIRCLE('',#4266,1.1);
#997=CIRCLE('',#4269,1.1);
#998=CIRCLE('',#4272,4.99999999999999);
#999=CIRCLE('',#4274,33.8);
#1000=CIRCLE('',#4280,33.8);
#1001=CIRCLE('',#4281,4.99999999999999);
#1002=CIRCLE('',#4282,1.1);
#1003=CIRCLE('',#4283,1.1);
#1004=CIRCLE('',#4285,1.1);
#1005=CIRCLE('',#4288,1.1);
#1006=CIRCLE('',#4291,4.99999999999999);
#1007=CIRCLE('',#4293,33.8);
#1008=CIRCLE('',#4299,33.8);
#1009=CIRCLE('',#4300,4.99999999999999);
#1010=CIRCLE('',#4301,1.1);
#1011=CIRCLE('',#4302,1.1);
#1012=CIRCLE('',#4304,1.1);
#1013=CIRCLE('',#4307,1.1);
#1014=CIRCLE('',#4310,4.99999999999999);
#1015=CIRCLE('',#4312,33.8);
#1016=CIRCLE('',#4318,33.8);
#1017=CIRCLE('',#4319,4.99999999999999);
#1018=CIRCLE('',#4320,1.1);
#1019=CIRCLE('',#4321,1.1);
#1020=CIRCLE('',#4323,1.1);
#1021=CIRCLE('',#4326,1.1);
#1022=CIRCLE('',#4329,4.99999999999999);
#1023=CIRCLE('',#4331,33.8);
#1024=CIRCLE('',#4337,33.8);
#1025=CIRCLE('',#4338,4.99999999999999);
#1026=CIRCLE('',#4339,1.1);
#1027=CIRCLE('',#4340,1.1);
#1028=CIRCLE('',#4342,1.1);
#1029=CIRCLE('',#4345,1.1);
#1030=CIRCLE('',#4348,4.99999999999999);
#1031=CIRCLE('',#4350,33.8);
#1032=LINE('',#5568,#1318);
#1033=LINE('',#5572,#1319);
#1034=LINE('',#5577,#1320);
#1035=LINE('',#5584,#1321);
#1036=LINE('',#5589,#1322);
#1037=LINE('',#5592,#1323);
#1038=LINE('',#5593,#1324);
#1039=LINE('',#5596,#1325);
#1040=LINE('',#5597,#1326);
#1041=LINE('',#5603,#1327);
#1042=LINE('',#5607,#1328);
#1043=LINE('',#5617,#1329);
#1044=LINE('',#5625,#1330);
#1045=LINE('',#5631,#1331);
#1046=LINE('',#5633,#1332);
#1047=LINE('',#5635,#1333);
#1048=LINE('',#5636,#1334);
#1049=LINE('',#5640,#1335);
#1050=LINE('',#5642,#1336);
#1051=LINE('',#5644,#1337);
#1052=LINE('',#5645,#1338);
#1053=LINE('',#5656,#1339);
#1054=LINE('',#5661,#1340);
#1055=LINE('',#5674,#1341);
#1056=LINE('',#5677,#1342);
#1057=LINE('',#5680,#1343);
#1058=LINE('',#5682,#1344);
#1059=LINE('',#5683,#1345);
#1060=LINE('',#5686,#1346);
#1061=LINE('',#5688,#1347);
#1062=LINE('',#5689,#1348);
#1063=LINE('',#5694,#1349);
#1064=LINE('',#5701,#1350);
#1065=LINE('',#5709,#1351);
#1066=LINE('',#5715,#1352);
#1067=LINE('',#5721,#1353);
#1068=LINE('',#5727,#1354);
#1069=LINE('',#5733,#1355);
#1070=LINE('',#5739,#1356);
#1071=LINE('',#5745,#1357);
#1072=LINE('',#5751,#1358);
#1073=LINE('',#5757,#1359);
#1074=LINE('',#5763,#1360);
#1075=LINE('',#5769,#1361);
#1076=LINE('',#5775,#1362);
#1077=LINE('',#5781,#1363);
#1078=LINE('',#5787,#1364);
#1079=LINE('',#5793,#1365);
#1080=LINE('',#5799,#1366);
#1081=LINE('',#5805,#1367);
#1082=LINE('',#5879,#1368);
#1083=LINE('',#5885,#1369);
#1084=LINE('',#5889,#1370);
#1085=LINE('',#5928,#1371);
#1086=LINE('',#5934,#1372);
#1087=LINE('',#5936,#1373);
#1088=LINE('',#5938,#1374);
#1089=LINE('',#5939,#1375);
#1090=LINE('',#5943,#1376);
#1091=LINE('',#5945,#1377);
#1092=LINE('',#5947,#1378);
#1093=LINE('',#5948,#1379);
#1094=LINE('',#5952,#1380);
#1095=LINE('',#5954,#1381);
#1096=LINE('',#5956,#1382);
#1097=LINE('',#5957,#1383);
#1098=LINE('',#5961,#1384);
#1099=LINE('',#5963,#1385);
#1100=LINE('',#5965,#1386);
#1101=LINE('',#5966,#1387);
#1102=LINE('',#5970,#1388);
#1103=LINE('',#5972,#1389);
#1104=LINE('',#5974,#1390);
#1105=LINE('',#5975,#1391);
#1106=LINE('',#5979,#1392);
#1107=LINE('',#5981,#1393);
#1108=LINE('',#5983,#1394);
#1109=LINE('',#5984,#1395);
#1110=LINE('',#5988,#1396);
#1111=LINE('',#5990,#1397);
#1112=LINE('',#5992,#1398);
#1113=LINE('',#5993,#1399);
#1114=LINE('',#5997,#1400);
#1115=LINE('',#5999,#1401);
#1116=LINE('',#6001,#1402);
#1117=LINE('',#6002,#1403);
#1118=LINE('',#6006,#1404);
#1119=LINE('',#6008,#1405);
#1120=LINE('',#6010,#1406);
#1121=LINE('',#6011,#1407);
#1122=LINE('',#6015,#1408);
#1123=LINE('',#6017,#1409);
#1124=LINE('',#6019,#1410);
#1125=LINE('',#6020,#1411);
#1126=LINE('',#6024,#1412);
#1127=LINE('',#6026,#1413);
#1128=LINE('',#6028,#1414);
#1129=LINE('',#6029,#1415);
#1130=LINE('',#6033,#1416);
#1131=LINE('',#6035,#1417);
#1132=LINE('',#6037,#1418);
#1133=LINE('',#6038,#1419);
#1134=LINE('',#6042,#1420);
#1135=LINE('',#6044,#1421);
#1136=LINE('',#6046,#1422);
#1137=LINE('',#6047,#1423);
#1138=LINE('',#6051,#1424);
#1139=LINE('',#6053,#1425);
#1140=LINE('',#6055,#1426);
#1141=LINE('',#6056,#1427);
#1142=LINE('',#6060,#1428);
#1143=LINE('',#6062,#1429);
#1144=LINE('',#6064,#1430);
#1145=LINE('',#6065,#1431);
#1146=LINE('',#6069,#1432);
#1147=LINE('',#6071,#1433);
#1148=LINE('',#6073,#1434);
#1149=LINE('',#6074,#1435);
#1150=LINE('',#6078,#1436);
#1151=LINE('',#6080,#1437);
#1152=LINE('',#6082,#1438);
#1153=LINE('',#6083,#1439);
#1154=LINE('',#6087,#1440);
#1155=LINE('',#6089,#1441);
#1156=LINE('',#6091,#1442);
#1157=LINE('',#6092,#1443);
#1158=LINE('',#6096,#1444);
#1159=LINE('',#6098,#1445);
#1160=LINE('',#6100,#1446);
#1161=LINE('',#6101,#1447);
#1162=LINE('',#6107,#1448);
#1163=LINE('',#6116,#1449);
#1164=LINE('',#6122,#1450);
#1165=LINE('',#6128,#1451);
#1166=LINE('',#6134,#1452);
#1167=LINE('',#6140,#1453);
#1168=LINE('',#6146,#1454);
#1169=LINE('',#6152,#1455);
#1170=LINE('',#6158,#1456);
#1171=LINE('',#6164,#1457);
#1172=LINE('',#6170,#1458);
#1173=LINE('',#6176,#1459);
#1174=LINE('',#6182,#1460);
#1175=LINE('',#6188,#1461);
#1176=LINE('',#6194,#1462);
#1177=LINE('',#6200,#1463);
#1178=LINE('',#6206,#1464);
#1179=LINE('',#6212,#1465);
#1180=LINE('',#6218,#1466);
#1181=LINE('',#6222,#1467);
#1182=LINE('',#6224,#1468);
#1183=LINE('',#6225,#1469);
#1184=LINE('',#6228,#1470);
#1185=LINE('',#6230,#1471);
#1186=LINE('',#6231,#1472);
#1187=LINE('',#6234,#1473);
#1188=LINE('',#6236,#1474);
#1189=LINE('',#6237,#1475);
#1190=LINE('',#6240,#1476);
#1191=LINE('',#6242,#1477);
#1192=LINE('',#6243,#1478);
#1193=LINE('',#6246,#1479);
#1194=LINE('',#6248,#1480);
#1195=LINE('',#6249,#1481);
#1196=LINE('',#6252,#1482);
#1197=LINE('',#6254,#1483);
#1198=LINE('',#6255,#1484);
#1199=LINE('',#6258,#1485);
#1200=LINE('',#6260,#1486);
#1201=LINE('',#6261,#1487);
#1202=LINE('',#6264,#1488);
#1203=LINE('',#6266,#1489);
#1204=LINE('',#6267,#1490);
#1205=LINE('',#6270,#1491);
#1206=LINE('',#6272,#1492);
#1207=LINE('',#6273,#1493);
#1208=LINE('',#6276,#1494);
#1209=LINE('',#6278,#1495);
#1210=LINE('',#6279,#1496);
#1211=LINE('',#6282,#1497);
#1212=LINE('',#6284,#1498);
#1213=LINE('',#6285,#1499);
#1214=LINE('',#6288,#1500);
#1215=LINE('',#6290,#1501);
#1216=LINE('',#6291,#1502);
#1217=LINE('',#6294,#1503);
#1218=LINE('',#6296,#1504);
#1219=LINE('',#6297,#1505);
#1220=LINE('',#6300,#1506);
#1221=LINE('',#6302,#1507);
#1222=LINE('',#6303,#1508);
#1223=LINE('',#6306,#1509);
#1224=LINE('',#6308,#1510);
#1225=LINE('',#6309,#1511);
#1226=LINE('',#6312,#1512);
#1227=LINE('',#6314,#1513);
#1228=LINE('',#6315,#1514);
#1229=LINE('',#6318,#1515);
#1230=LINE('',#6320,#1516);
#1231=LINE('',#6321,#1517);
#1232=LINE('',#6324,#1518);
#1233=LINE('',#6326,#1519);
#1234=LINE('',#6327,#1520);
#1235=LINE('',#6330,#1521);
#1236=LINE('',#6332,#1522);
#1237=LINE('',#6333,#1523);
#1238=LINE('',#6337,#1524);
#1239=LINE('',#6345,#1525);
#1240=LINE('',#6349,#1526);
#1241=LINE('',#6368,#1527);
#1242=LINE('',#6381,#1528);
#1243=LINE('',#6409,#1529);
#1244=LINE('',#6410,#1530);
#1245=LINE('',#6413,#1531);
#1246=LINE('',#6416,#1532);
#1247=LINE('',#6420,#1533);
#1248=LINE('',#6428,#1534);
#1249=LINE('',#6430,#1535);
#1250=LINE('',#6432,#1536);
#1251=LINE('',#6433,#1537);
#1252=LINE('',#6437,#1538);
#1253=LINE('',#6439,#1539);
#1254=LINE('',#6441,#1540);
#1255=LINE('',#6442,#1541);
#1256=LINE('',#6453,#1542);
#1257=LINE('',#6458,#1543);
#1258=LINE('',#6469,#1544);
#1259=LINE('',#6471,#1545);
#1260=LINE('',#6473,#1546);
#1261=LINE('',#6474,#1547);
#1262=LINE('',#6478,#1548);
#1263=LINE('',#6480,#1549);
#1264=LINE('',#6482,#1550);
#1265=LINE('',#6483,#1551);
#1266=LINE('',#6494,#1552);
#1267=LINE('',#6499,#1553);
#1268=LINE('',#6510,#1554);
#1269=LINE('',#6512,#1555);
#1270=LINE('',#6514,#1556);
#1271=LINE('',#6515,#1557);
#1272=LINE('',#6519,#1558);
#1273=LINE('',#6521,#1559);
#1274=LINE('',#6523,#1560);
#1275=LINE('',#6524,#1561);
#1276=LINE('',#6535,#1562);
#1277=LINE('',#6540,#1563);
#1278=LINE('',#6551,#1564);
#1279=LINE('',#6553,#1565);
#1280=LINE('',#6555,#1566);
#1281=LINE('',#6556,#1567);
#1282=LINE('',#6560,#1568);
#1283=LINE('',#6562,#1569);
#1284=LINE('',#6564,#1570);
#1285=LINE('',#6565,#1571);
#1286=LINE('',#6576,#1572);
#1287=LINE('',#6581,#1573);
#1288=LINE('',#6592,#1574);
#1289=LINE('',#6594,#1575);
#1290=LINE('',#6596,#1576);
#1291=LINE('',#6597,#1577);
#1292=LINE('',#6601,#1578);
#1293=LINE('',#6603,#1579);
#1294=LINE('',#6605,#1580);
#1295=LINE('',#6606,#1581);
#1296=LINE('',#6617,#1582);
#1297=LINE('',#6622,#1583);
#1298=LINE('',#6633,#1584);
#1299=LINE('',#6635,#1585);
#1300=LINE('',#6637,#1586);
#1301=LINE('',#6638,#1587);
#1302=LINE('',#6642,#1588);
#1303=LINE('',#6644,#1589);
#1304=LINE('',#6646,#1590);
#1305=LINE('',#6647,#1591);
#1306=LINE('',#6658,#1592);
#1307=LINE('',#6663,#1593);
#1308=LINE('',#6674,#1594);
#1309=LINE('',#6676,#1595);
#1310=LINE('',#6678,#1596);
#1311=LINE('',#6679,#1597);
#1312=LINE('',#6683,#1598);
#1313=LINE('',#6685,#1599);
#1314=LINE('',#6687,#1600);
#1315=LINE('',#6688,#1601);
#1316=LINE('',#6699,#1602);
#1317=LINE('',#6704,#1603);
#1318=VECTOR('',#4371,10.);
#1319=VECTOR('',#4374,35.);
#1320=VECTOR('',#4379,10.);
#1321=VECTOR('',#4388,10.);
#1322=VECTOR('',#4393,10.);
#1323=VECTOR('',#4396,10.);
#1324=VECTOR('',#4397,10.);
#1325=VECTOR('',#4400,10.);
#1326=VECTOR('',#4401,10.);
#1327=VECTOR('',#4410,33.);
#1328=VECTOR('',#4415,40.);
#1329=VECTOR('',#4428,1.25);
#1330=VECTOR('',#4439,0.75);
#1331=VECTOR('',#4446,10.);
#1332=VECTOR('',#4447,10.);
#1333=VECTOR('',#4448,10.);
#1334=VECTOR('',#4449,10.);
#1335=VECTOR('',#4452,10.);
#1336=VECTOR('',#4453,10.);
#1337=VECTOR('',#4454,10.);
#1338=VECTOR('',#4455,10.);
#1339=VECTOR('',#4470,1.1);
#1340=VECTOR('',#4477,1.1);
#1341=VECTOR('',#4496,10.);
#1342=VECTOR('',#4499,10.);
#1343=VECTOR('',#4502,10.);
#1344=VECTOR('',#4503,10.);
#1345=VECTOR('',#4504,10.);
#1346=VECTOR('',#4507,10.);
#1347=VECTOR('',#4508,10.);
#1348=VECTOR('',#4509,10.);
#1349=VECTOR('',#4514,34.);
#1350=VECTOR('',#4523,35.);
#1351=VECTOR('',#4534,1.1);
#1352=VECTOR('',#4541,1.1);
#1353=VECTOR('',#4548,25.);
#1354=VECTOR('',#4555,1.1);
#1355=VECTOR('',#4562,1.1);
#1356=VECTOR('',#4569,1.1);
#1357=VECTOR('',#4576,1.1);
#1358=VECTOR('',#4583,1.1);
#1359=VECTOR('',#4590,1.1);
#1360=VECTOR('',#4597,1.1);
#1361=VECTOR('',#4604,1.1);
#1362=VECTOR('',#4611,1.1);
#1363=VECTOR('',#4618,1.1);
#1364=VECTOR('',#4625,1.1);
#1365=VECTOR('',#4632,1.1);
#1366=VECTOR('',#4639,1.1);
#1367=VECTOR('',#4646,1.1);
#1368=VECTOR('',#4681,5.5);
#1369=VECTOR('',#4688,6.);
#1370=VECTOR('',#4695,5.51285218418961);
#1371=VECTOR('',#4700,0.75);
#1372=VECTOR('',#4707,10.);
#1373=VECTOR('',#4708,10.);
#1374=VECTOR('',#4709,10.);
#1375=VECTOR('',#4710,10.);
#1376=VECTOR('',#4713,10.);
#1377=VECTOR('',#4714,10.);
#1378=VECTOR('',#4715,10.);
#1379=VECTOR('',#4716,10.);
#1380=VECTOR('',#4719,10.);
#1381=VECTOR('',#4720,10.);
#1382=VECTOR('',#4721,10.);
#1383=VECTOR('',#4722,10.);
#1384=VECTOR('',#4725,10.);
#1385=VECTOR('',#4726,10.);
#1386=VECTOR('',#4727,10.);
#1387=VECTOR('',#4728,10.);
#1388=VECTOR('',#4731,10.);
#1389=VECTOR('',#4732,10.);
#1390=VECTOR('',#4733,10.);
#1391=VECTOR('',#4734,10.);
#1392=VECTOR('',#4737,10.);
#1393=VECTOR('',#4738,10.);
#1394=VECTOR('',#4739,10.);
#1395=VECTOR('',#4740,10.);
#1396=VECTOR('',#4743,10.);
#1397=VECTOR('',#4744,10.);
#1398=VECTOR('',#4745,10.);
#1399=VECTOR('',#4746,10.);
#1400=VECTOR('',#4749,10.);
#1401=VECTOR('',#4750,10.);
#1402=VECTOR('',#4751,10.);
#1403=VECTOR('',#4752,10.);
#1404=VECTOR('',#4755,10.);
#1405=VECTOR('',#4756,10.);
#1406=VECTOR('',#4757,10.);
#1407=VECTOR('',#4758,10.);
#1408=VECTOR('',#4761,10.);
#1409=VECTOR('',#4762,10.);
#1410=VECTOR('',#4763,10.);
#1411=VECTOR('',#4764,10.);
#1412=VECTOR('',#4767,10.);
#1413=VECTOR('',#4768,10.);
#1414=VECTOR('',#4769,10.);
#1415=VECTOR('',#4770,10.);
#1416=VECTOR('',#4773,10.);
#1417=VECTOR('',#4774,10.);
#1418=VECTOR('',#4775,10.);
#1419=VECTOR('',#4776,10.);
#1420=VECTOR('',#4779,10.);
#1421=VECTOR('',#4780,10.);
#1422=VECTOR('',#4781,10.);
#1423=VECTOR('',#4782,10.);
#1424=VECTOR('',#4785,10.);
#1425=VECTOR('',#4786,10.);
#1426=VECTOR('',#4787,10.);
#1427=VECTOR('',#4788,10.);
#1428=VECTOR('',#4791,10.);
#1429=VECTOR('',#4792,10.);
#1430=VECTOR('',#4793,10.);
#1431=VECTOR('',#4794,10.);
#1432=VECTOR('',#4797,10.);
#1433=VECTOR('',#4798,10.);
#1434=VECTOR('',#4799,10.);
#1435=VECTOR('',#4800,10.);
#1436=VECTOR('',#4803,10.);
#1437=VECTOR('',#4804,10.);
#1438=VECTOR('',#4805,10.);
#1439=VECTOR('',#4806,10.);
#1440=VECTOR('',#4809,10.);
#1441=VECTOR('',#4810,10.);
#1442=VECTOR('',#4811,10.);
#1443=VECTOR('',#4812,10.);
#1444=VECTOR('',#4815,10.);
#1445=VECTOR('',#4816,10.);
#1446=VECTOR('',#4817,10.);
#1447=VECTOR('',#4818,10.);
#1448=VECTOR('',#4823,10.);
#1449=VECTOR('',#4834,10.);
#1450=VECTOR('',#4841,10.);
#1451=VECTOR('',#4848,10.);
#1452=VECTOR('',#4855,10.);
#1453=VECTOR('',#4862,10.);
#1454=VECTOR('',#4869,10.);
#1455=VECTOR('',#4876,10.);
#1456=VECTOR('',#4883,10.);
#1457=VECTOR('',#4890,10.);
#1458=VECTOR('',#4897,10.);
#1459=VECTOR('',#4904,10.);
#1460=VECTOR('',#4911,10.);
#1461=VECTOR('',#4918,10.);
#1462=VECTOR('',#4925,10.);
#1463=VECTOR('',#4932,10.);
#1464=VECTOR('',#4939,10.);
#1465=VECTOR('',#4946,10.);
#1466=VECTOR('',#4953,10.);
#1467=VECTOR('',#4958,10.);
#1468=VECTOR('',#4959,10.);
#1469=VECTOR('',#4960,10.);
#1470=VECTOR('',#4963,10.);
#1471=VECTOR('',#4964,10.);
#1472=VECTOR('',#4965,10.);
#1473=VECTOR('',#4968,10.);
#1474=VECTOR('',#4969,10.);
#1475=VECTOR('',#4970,10.);
#1476=VECTOR('',#4973,10.);
#1477=VECTOR('',#4974,10.);
#1478=VECTOR('',#4975,10.);
#1479=VECTOR('',#4978,10.);
#1480=VECTOR('',#4979,10.);
#1481=VECTOR('',#4980,10.);
#1482=VECTOR('',#4983,10.);
#1483=VECTOR('',#4984,10.);
#1484=VECTOR('',#4985,10.);
#1485=VECTOR('',#4988,10.);
#1486=VECTOR('',#4989,10.);
#1487=VECTOR('',#4990,10.);
#1488=VECTOR('',#4993,10.);
#1489=VECTOR('',#4994,10.);
#1490=VECTOR('',#4995,10.);
#1491=VECTOR('',#4998,10.);
#1492=VECTOR('',#4999,10.);
#1493=VECTOR('',#5000,10.);
#1494=VECTOR('',#5003,10.);
#1495=VECTOR('',#5004,10.);
#1496=VECTOR('',#5005,10.);
#1497=VECTOR('',#5008,10.);
#1498=VECTOR('',#5009,10.);
#1499=VECTOR('',#5010,10.);
#1500=VECTOR('',#5013,10.);
#1501=VECTOR('',#5014,10.);
#1502=VECTOR('',#5015,10.);
#1503=VECTOR('',#5018,10.);
#1504=VECTOR('',#5019,10.);
#1505=VECTOR('',#5020,10.);
#1506=VECTOR('',#5023,10.);
#1507=VECTOR('',#5024,10.);
#1508=VECTOR('',#5025,10.);
#1509=VECTOR('',#5028,10.);
#1510=VECTOR('',#5029,10.);
#1511=VECTOR('',#5030,10.);
#1512=VECTOR('',#5033,10.);
#1513=VECTOR('',#5034,10.);
#1514=VECTOR('',#5035,10.);
#1515=VECTOR('',#5038,10.);
#1516=VECTOR('',#5039,10.);
#1517=VECTOR('',#5040,10.);
#1518=VECTOR('',#5043,10.);
#1519=VECTOR('',#5044,10.);
#1520=VECTOR('',#5045,10.);
#1521=VECTOR('',#5048,10.);
#1522=VECTOR('',#5049,10.);
#1523=VECTOR('',#5050,10.);
#1524=VECTOR('',#5055,25.);
#1525=VECTOR('',#5066,10.);
#1526=VECTOR('',#5069,10.);
#1527=VECTOR('',#5104,10.);
#1528=VECTOR('',#5127,10.);
#1529=VECTOR('',#5180,10.);
#1530=VECTOR('',#5181,10.);
#1531=VECTOR('',#5184,10.);
#1532=VECTOR('',#5189,10.);
#1533=VECTOR('',#5194,34.);
#1534=VECTOR('',#5205,10.);
#1535=VECTOR('',#5206,10.);
#1536=VECTOR('',#5207,10.);
#1537=VECTOR('',#5208,10.);
#1538=VECTOR('',#5211,10.);
#1539=VECTOR('',#5212,10.);
#1540=VECTOR('',#5213,10.);
#1541=VECTOR('',#5214,10.);
#1542=VECTOR('',#5229,1.1);
#1543=VECTOR('',#5236,1.1);
#1544=VECTOR('',#5253,10.);
#1545=VECTOR('',#5254,10.);
#1546=VECTOR('',#5255,10.);
#1547=VECTOR('',#5256,10.);
#1548=VECTOR('',#5259,10.);
#1549=VECTOR('',#5260,10.);
#1550=VECTOR('',#5261,10.);
#1551=VECTOR('',#5262,10.);
#1552=VECTOR('',#5277,1.1);
#1553=VECTOR('',#5284,1.1);
#1554=VECTOR('',#5301,10.);
#1555=VECTOR('',#5302,10.);
#1556=VECTOR('',#5303,10.);
#1557=VECTOR('',#5304,10.);
#1558=VECTOR('',#5307,10.);
#1559=VECTOR('',#5308,10.);
#1560=VECTOR('',#5309,10.);
#1561=VECTOR('',#5310,10.);
#1562=VECTOR('',#5325,1.1);
#1563=VECTOR('',#5332,1.1);
#1564=VECTOR('',#5349,10.);
#1565=VECTOR('',#5350,10.);
#1566=VECTOR('',#5351,10.);
#1567=VECTOR('',#5352,10.);
#1568=VECTOR('',#5355,10.);
#1569=VECTOR('',#5356,10.);
#1570=VECTOR('',#5357,10.);
#1571=VECTOR('',#5358,10.);
#1572=VECTOR('',#5373,1.1);
#1573=VECTOR('',#5380,1.1);
#1574=VECTOR('',#5397,10.);
#1575=VECTOR('',#5398,10.);
#1576=VECTOR('',#5399,10.);
#1577=VECTOR('',#5400,10.);
#1578=VECTOR('',#5403,10.);
#1579=VECTOR('',#5404,10.);
#1580=VECTOR('',#5405,10.);
#1581=VECTOR('',#5406,10.);
#1582=VECTOR('',#5421,1.1);
#1583=VECTOR('',#5428,1.1);
#1584=VECTOR('',#5445,10.);
#1585=VECTOR('',#5446,10.);
#1586=VECTOR('',#5447,10.);
#1587=VECTOR('',#5448,10.);
#1588=VECTOR('',#5451,10.);
#1589=VECTOR('',#5452,10.);
#1590=VECTOR('',#5453,10.);
#1591=VECTOR('',#5454,10.);
#1592=VECTOR('',#5469,1.1);
#1593=VECTOR('',#5476,1.1);
#1594=VECTOR('',#5493,10.);
#1595=VECTOR('',#5494,10.);
#1596=VECTOR('',#5495,10.);
#1597=VECTOR('',#5496,10.);
#1598=VECTOR('',#5499,10.);
#1599=VECTOR('',#5500,10.);
#1600=VECTOR('',#5501,10.);
#1601=VECTOR('',#5502,10.);
#1602=VECTOR('',#5517,1.1);
#1603=VECTOR('',#5524,1.1);
#1604=VERTEX_POINT('',#5566);
#1605=VERTEX_POINT('',#5567);
#1606=VERTEX_POINT('',#5569);
#1607=VERTEX_POINT('',#5571);
#1608=VERTEX_POINT('',#5574);
#1609=VERTEX_POINT('',#5576);
#1610=VERTEX_POINT('',#5580);
#1611=VERTEX_POINT('',#5583);
#1612=VERTEX_POINT('',#5585);
#1613=VERTEX_POINT('',#5587);
#1614=VERTEX_POINT('',#5591);
#1615=VERTEX_POINT('',#5595);
#1616=VERTEX_POINT('',#5601);
#1617=VERTEX_POINT('',#5605);
#1618=VERTEX_POINT('',#5611);
#1619=VERTEX_POINT('',#5613);
#1620=VERTEX_POINT('',#5616);
#1621=VERTEX_POINT('',#5620);
#1622=VERTEX_POINT('',#5623);
#1623=VERTEX_POINT('',#5629);
#1624=VERTEX_POINT('',#5630);
#1625=VERTEX_POINT('',#5632);
#1626=VERTEX_POINT('',#5634);
#1627=VERTEX_POINT('',#5638);
#1628=VERTEX_POINT('',#5639);
#1629=VERTEX_POINT('',#5641);
#1630=VERTEX_POINT('',#5643);
#1631=VERTEX_POINT('',#5649);
#1632=VERTEX_POINT('',#5651);
#1633=VERTEX_POINT('',#5654);
#1634=VERTEX_POINT('',#5659);
#1635=VERTEX_POINT('',#5670);
#1636=VERTEX_POINT('',#5671);
#1637=VERTEX_POINT('',#5673);
#1638=VERTEX_POINT('',#5675);
#1639=VERTEX_POINT('',#5679);
#1640=VERTEX_POINT('',#5681);
#1641=VERTEX_POINT('',#5685);
#1642=VERTEX_POINT('',#5687);
#1643=VERTEX_POINT('',#5691);
#1644=VERTEX_POINT('',#5693);
#1645=VERTEX_POINT('',#5698);
#1646=VERTEX_POINT('',#5700);
#1647=VERTEX_POINT('',#5706);
#1648=VERTEX_POINT('',#5708);
#1649=VERTEX_POINT('',#5712);
#1650=VERTEX_POINT('',#5714);
#1651=VERTEX_POINT('',#5718);
#1652=VERTEX_POINT('',#5720);
#1653=VERTEX_POINT('',#5724);
#1654=VERTEX_POINT('',#5726);
#1655=VERTEX_POINT('',#5730);
#1656=VERTEX_POINT('',#5732);
#1657=VERTEX_POINT('',#5736);
#1658=VERTEX_POINT('',#5738);
#1659=VERTEX_POINT('',#5742);
#1660=VERTEX_POINT('',#5744);
#1661=VERTEX_POINT('',#5748);
#1662=VERTEX_POINT('',#5750);
#1663=VERTEX_POINT('',#5754);
#1664=VERTEX_POINT('',#5756);
#1665=VERTEX_POINT('',#5760);
#1666=VERTEX_POINT('',#5762);
#1667=VERTEX_POINT('',#5766);
#1668=VERTEX_POINT('',#5768);
#1669=VERTEX_POINT('',#5772);
#1670=VERTEX_POINT('',#5774);
#1671=VERTEX_POINT('',#5778);
#1672=VERTEX_POINT('',#5780);
#1673=VERTEX_POINT('',#5784);
#1674=VERTEX_POINT('',#5786);
#1675=VERTEX_POINT('',#5790);
#1676=VERTEX_POINT('',#5792);
#1677=VERTEX_POINT('',#5796);
#1678=VERTEX_POINT('',#5798);
#1679=VERTEX_POINT('',#5802);
#1680=VERTEX_POINT('',#5804);
#1681=VERTEX_POINT('',#5811);
#1682=VERTEX_POINT('',#5812);
#1683=VERTEX_POINT('',#5816);
#1684=VERTEX_POINT('',#5818);
#1685=VERTEX_POINT('',#5824);
#1686=VERTEX_POINT('',#5825);
#1687=VERTEX_POINT('',#5834);
#1688=VERTEX_POINT('',#5836);
#1689=VERTEX_POINT('',#5862);
#1690=VERTEX_POINT('',#5866);
#1691=VERTEX_POINT('',#5876);
#1692=VERTEX_POINT('',#5878);
#1693=VERTEX_POINT('',#5880);
#1694=VERTEX_POINT('',#5884);
#1695=VERTEX_POINT('',#5892);
#1696=VERTEX_POINT('',#5927);
#1697=VERTEX_POINT('',#5932);
#1698=VERTEX_POINT('',#5933);
#1699=VERTEX_POINT('',#5935);
#1700=VERTEX_POINT('',#5937);
#1701=VERTEX_POINT('',#5941);
#1702=VERTEX_POINT('',#5942);
#1703=VERTEX_POINT('',#5944);
#1704=VERTEX_POINT('',#5946);
#1705=VERTEX_POINT('',#5950);
#1706=VERTEX_POINT('',#5951);
#1707=VERTEX_POINT('',#5953);
#1708=VERTEX_POINT('',#5955);
#1709=VERTEX_POINT('',#5959);
#1710=VERTEX_POINT('',#5960);
#1711=VERTEX_POINT('',#5962);
#1712=VERTEX_POINT('',#5964);
#1713=VERTEX_POINT('',#5968);
#1714=VERTEX_POINT('',#5969);
#1715=VERTEX_POINT('',#5971);
#1716=VERTEX_POINT('',#5973);
#1717=VERTEX_POINT('',#5977);
#1718=VERTEX_POINT('',#5978);
#1719=VERTEX_POINT('',#5980);
#1720=VERTEX_POINT('',#5982);
#1721=VERTEX_POINT('',#5986);
#1722=VERTEX_POINT('',#5987);
#1723=VERTEX_POINT('',#5989);
#1724=VERTEX_POINT('',#5991);
#1725=VERTEX_POINT('',#5995);
#1726=VERTEX_POINT('',#5996);
#1727=VERTEX_POINT('',#5998);
#1728=VERTEX_POINT('',#6000);
#1729=VERTEX_POINT('',#6004);
#1730=VERTEX_POINT('',#6005);
#1731=VERTEX_POINT('',#6007);
#1732=VERTEX_POINT('',#6009);
#1733=VERTEX_POINT('',#6013);
#1734=VERTEX_POINT('',#6014);
#1735=VERTEX_POINT('',#6016);
#1736=VERTEX_POINT('',#6018);
#1737=VERTEX_POINT('',#6022);
#1738=VERTEX_POINT('',#6023);
#1739=VERTEX_POINT('',#6025);
#1740=VERTEX_POINT('',#6027);
#1741=VERTEX_POINT('',#6031);
#1742=VERTEX_POINT('',#6032);
#1743=VERTEX_POINT('',#6034);
#1744=VERTEX_POINT('',#6036);
#1745=VERTEX_POINT('',#6040);
#1746=VERTEX_POINT('',#6041);
#1747=VERTEX_POINT('',#6043);
#1748=VERTEX_POINT('',#6045);
#1749=VERTEX_POINT('',#6049);
#1750=VERTEX_POINT('',#6050);
#1751=VERTEX_POINT('',#6052);
#1752=VERTEX_POINT('',#6054);
#1753=VERTEX_POINT('',#6058);
#1754=VERTEX_POINT('',#6059);
#1755=VERTEX_POINT('',#6061);
#1756=VERTEX_POINT('',#6063);
#1757=VERTEX_POINT('',#6067);
#1758=VERTEX_POINT('',#6068);
#1759=VERTEX_POINT('',#6070);
#1760=VERTEX_POINT('',#6072);
#1761=VERTEX_POINT('',#6076);
#1762=VERTEX_POINT('',#6077);
#1763=VERTEX_POINT('',#6079);
#1764=VERTEX_POINT('',#6081);
#1765=VERTEX_POINT('',#6085);
#1766=VERTEX_POINT('',#6086);
#1767=VERTEX_POINT('',#6088);
#1768=VERTEX_POINT('',#6090);
#1769=VERTEX_POINT('',#6094);
#1770=VERTEX_POINT('',#6095);
#1771=VERTEX_POINT('',#6097);
#1772=VERTEX_POINT('',#6099);
#1773=VERTEX_POINT('',#6103);
#1774=VERTEX_POINT('',#6104);
#1775=VERTEX_POINT('',#6106);
#1776=VERTEX_POINT('',#6108);
#1777=VERTEX_POINT('',#6113);
#1778=VERTEX_POINT('',#6115);
#1779=VERTEX_POINT('',#6119);
#1780=VERTEX_POINT('',#6121);
#1781=VERTEX_POINT('',#6125);
#1782=VERTEX_POINT('',#6127);
#1783=VERTEX_POINT('',#6131);
#1784=VERTEX_POINT('',#6133);
#1785=VERTEX_POINT('',#6137);
#1786=VERTEX_POINT('',#6139);
#1787=VERTEX_POINT('',#6143);
#1788=VERTEX_POINT('',#6145);
#1789=VERTEX_POINT('',#6149);
#1790=VERTEX_POINT('',#6151);
#1791=VERTEX_POINT('',#6155);
#1792=VERTEX_POINT('',#6157);
#1793=VERTEX_POINT('',#6161);
#1794=VERTEX_POINT('',#6163);
#1795=VERTEX_POINT('',#6167);
#1796=VERTEX_POINT('',#6169);
#1797=VERTEX_POINT('',#6173);
#1798=VERTEX_POINT('',#6175);
#1799=VERTEX_POINT('',#6179);
#1800=VERTEX_POINT('',#6181);
#1801=VERTEX_POINT('',#6185);
#1802=VERTEX_POINT('',#6187);
#1803=VERTEX_POINT('',#6191);
#1804=VERTEX_POINT('',#6193);
#1805=VERTEX_POINT('',#6197);
#1806=VERTEX_POINT('',#6199);
#1807=VERTEX_POINT('',#6203);
#1808=VERTEX_POINT('',#6205);
#1809=VERTEX_POINT('',#6209);
#1810=VERTEX_POINT('',#6211);
#1811=VERTEX_POINT('',#6215);
#1812=VERTEX_POINT('',#6217);
#1813=VERTEX_POINT('',#6221);
#1814=VERTEX_POINT('',#6223);
#1815=VERTEX_POINT('',#6227);
#1816=VERTEX_POINT('',#6229);
#1817=VERTEX_POINT('',#6233);
#1818=VERTEX_POINT('',#6235);
#1819=VERTEX_POINT('',#6239);
#1820=VERTEX_POINT('',#6241);
#1821=VERTEX_POINT('',#6245);
#1822=VERTEX_POINT('',#6247);
#1823=VERTEX_POINT('',#6251);
#1824=VERTEX_POINT('',#6253);
#1825=VERTEX_POINT('',#6257);
#1826=VERTEX_POINT('',#6259);
#1827=VERTEX_POINT('',#6263);
#1828=VERTEX_POINT('',#6265);
#1829=VERTEX_POINT('',#6269);
#1830=VERTEX_POINT('',#6271);
#1831=VERTEX_POINT('',#6275);
#1832=VERTEX_POINT('',#6277);
#1833=VERTEX_POINT('',#6281);
#1834=VERTEX_POINT('',#6283);
#1835=VERTEX_POINT('',#6287);
#1836=VERTEX_POINT('',#6289);
#1837=VERTEX_POINT('',#6293);
#1838=VERTEX_POINT('',#6295);
#1839=VERTEX_POINT('',#6299);
#1840=VERTEX_POINT('',#6301);
#1841=VERTEX_POINT('',#6305);
#1842=VERTEX_POINT('',#6307);
#1843=VERTEX_POINT('',#6311);
#1844=VERTEX_POINT('',#6313);
#1845=VERTEX_POINT('',#6317);
#1846=VERTEX_POINT('',#6319);
#1847=VERTEX_POINT('',#6323);
#1848=VERTEX_POINT('',#6325);
#1849=VERTEX_POINT('',#6329);
#1850=VERTEX_POINT('',#6331);
#1851=VERTEX_POINT('',#6335);
#1852=VERTEX_POINT('',#6342);
#1853=VERTEX_POINT('',#6344);
#1854=VERTEX_POINT('',#6346);
#1855=VERTEX_POINT('',#6348);
#1856=VERTEX_POINT('',#6366);
#1857=VERTEX_POINT('',#6380);
#1858=VERTEX_POINT('',#6408);
#1859=VERTEX_POINT('',#6412);
#1860=VERTEX_POINT('',#6418);
#1861=VERTEX_POINT('',#6426);
#1862=VERTEX_POINT('',#6427);
#1863=VERTEX_POINT('',#6429);
#1864=VERTEX_POINT('',#6431);
#1865=VERTEX_POINT('',#6435);
#1866=VERTEX_POINT('',#6436);
#1867=VERTEX_POINT('',#6438);
#1868=VERTEX_POINT('',#6440);
#1869=VERTEX_POINT('',#6446);
#1870=VERTEX_POINT('',#6448);
#1871=VERTEX_POINT('',#6451);
#1872=VERTEX_POINT('',#6456);
#1873=VERTEX_POINT('',#6467);
#1874=VERTEX_POINT('',#6468);
#1875=VERTEX_POINT('',#6470);
#1876=VERTEX_POINT('',#6472);
#1877=VERTEX_POINT('',#6476);
#1878=VERTEX_POINT('',#6477);
#1879=VERTEX_POINT('',#6479);
#1880=VERTEX_POINT('',#6481);
#1881=VERTEX_POINT('',#6487);
#1882=VERTEX_POINT('',#6489);
#1883=VERTEX_POINT('',#6492);
#1884=VERTEX_POINT('',#6497);
#1885=VERTEX_POINT('',#6508);
#1886=VERTEX_POINT('',#6509);
#1887=VERTEX_POINT('',#6511);
#1888=VERTEX_POINT('',#6513);
#1889=VERTEX_POINT('',#6517);
#1890=VERTEX_POINT('',#6518);
#1891=VERTEX_POINT('',#6520);
#1892=VERTEX_POINT('',#6522);
#1893=VERTEX_POINT('',#6528);
#1894=VERTEX_POINT('',#6530);
#1895=VERTEX_POINT('',#6533);
#1896=VERTEX_POINT('',#6538);
#1897=VERTEX_POINT('',#6549);
#1898=VERTEX_POINT('',#6550);
#1899=VERTEX_POINT('',#6552);
#1900=VERTEX_POINT('',#6554);
#1901=VERTEX_POINT('',#6558);
#1902=VERTEX_POINT('',#6559);
#1903=VERTEX_POINT('',#6561);
#1904=VERTEX_POINT('',#6563);
#1905=VERTEX_POINT('',#6569);
#1906=VERTEX_POINT('',#6571);
#1907=VERTEX_POINT('',#6574);
#1908=VERTEX_POINT('',#6579);
#1909=VERTEX_POINT('',#6590);
#1910=VERTEX_POINT('',#6591);
#1911=VERTEX_POINT('',#6593);
#1912=VERTEX_POINT('',#6595);
#1913=VERTEX_POINT('',#6599);
#1914=VERTEX_POINT('',#6600);
#1915=VERTEX_POINT('',#6602);
#1916=VERTEX_POINT('',#6604);
#1917=VERTEX_POINT('',#6610);
#1918=VERTEX_POINT('',#6612);
#1919=VERTEX_POINT('',#6615);
#1920=VERTEX_POINT('',#6620);
#1921=VERTEX_POINT('',#6631);
#1922=VERTEX_POINT('',#6632);
#1923=VERTEX_POINT('',#6634);
#1924=VERTEX_POINT('',#6636);
#1925=VERTEX_POINT('',#6640);
#1926=VERTEX_POINT('',#6641);
#1927=VERTEX_POINT('',#6643);
#1928=VERTEX_POINT('',#6645);
#1929=VERTEX_POINT('',#6651);
#1930=VERTEX_POINT('',#6653);
#1931=VERTEX_POINT('',#6656);
#1932=VERTEX_POINT('',#6661);
#1933=VERTEX_POINT('',#6672);
#1934=VERTEX_POINT('',#6673);
#1935=VERTEX_POINT('',#6675);
#1936=VERTEX_POINT('',#6677);
#1937=VERTEX_POINT('',#6681);
#1938=VERTEX_POINT('',#6682);
#1939=VERTEX_POINT('',#6684);
#1940=VERTEX_POINT('',#6686);
#1941=VERTEX_POINT('',#6692);
#1942=VERTEX_POINT('',#6694);
#1943=VERTEX_POINT('',#6697);
#1944=VERTEX_POINT('',#6702);
#1945=EDGE_CURVE('',#1604,#1605,#1032,.T.);
#1946=EDGE_CURVE('',#1606,#1604,#816,.T.);
#1947=EDGE_CURVE('',#1606,#1607,#1033,.T.);
#1948=EDGE_CURVE('',#1607,#1607,#817,.T.);
#1949=EDGE_CURVE('',#1608,#1606,#818,.T.);
#1950=EDGE_CURVE('',#1608,#1609,#1034,.T.);
#1951=EDGE_CURVE('',#1609,#1605,#819,.T.);
#1952=EDGE_CURVE('',#1610,#1610,#820,.T.);
#1953=EDGE_CURVE('',#1604,#1611,#1035,.T.);
#1954=EDGE_CURVE('',#1611,#1612,#821,.T.);
#1955=EDGE_CURVE('',#1612,#1613,#822,.T.);
#1956=EDGE_CURVE('',#1613,#1608,#1036,.T.);
#1957=EDGE_CURVE('',#1614,#1613,#1037,.T.);
#1958=EDGE_CURVE('',#1614,#1609,#1038,.T.);
#1959=EDGE_CURVE('',#1605,#1615,#1039,.T.);
#1960=EDGE_CURVE('',#1611,#1615,#1040,.T.);
#1961=EDGE_CURVE('',#1615,#1614,#823,.T.);
#1962=EDGE_CURVE('',#1616,#1616,#824,.T.);
#1963=EDGE_CURVE('',#1616,#1610,#1041,.T.);
#1964=EDGE_CURVE('',#1617,#1617,#825,.T.);
#1965=EDGE_CURVE('',#1617,#1612,#1042,.T.);
#1966=EDGE_CURVE('',#1618,#1618,#826,.T.);
#1967=EDGE_CURVE('',#1619,#1618,#827,.T.);
#1968=EDGE_CURVE('',#1618,#1620,#1043,.T.);
#1969=EDGE_CURVE('',#1620,#1620,#828,.T.);
#1970=EDGE_CURVE('',#1621,#1621,#829,.T.);
#1971=EDGE_CURVE('',#1622,#1622,#830,.T.);
#1972=EDGE_CURVE('',#1622,#1621,#1044,.T.);
#1973=EDGE_CURVE('',#1623,#1624,#1045,.T.);
#1974=EDGE_CURVE('',#1625,#1623,#1046,.T.);
#1975=EDGE_CURVE('',#1626,#1625,#1047,.T.);
#1976=EDGE_CURVE('',#1624,#1626,#1048,.T.);
#1977=EDGE_CURVE('',#1627,#1628,#1049,.T.);
#1978=EDGE_CURVE('',#1629,#1627,#1050,.T.);
#1979=EDGE_CURVE('',#1630,#1629,#1051,.T.);
#1980=EDGE_CURVE('',#1628,#1630,#1052,.T.);
#1981=EDGE_CURVE('',#1627,#1624,#831,.T.);
#1982=EDGE_CURVE('',#1623,#1628,#832,.T.);
#1983=EDGE_CURVE('',#1631,#1631,#833,.T.);
#1984=EDGE_CURVE('',#1632,#1632,#834,.T.);
#1985=EDGE_CURVE('',#1633,#1633,#835,.T.);
#1986=EDGE_CURVE('',#1633,#1631,#1053,.T.);
#1987=EDGE_CURVE('',#1634,#1634,#836,.T.);
#1988=EDGE_CURVE('',#1634,#1632,#1054,.T.);
#1989=EDGE_CURVE('',#1625,#1630,#837,.T.);
#1990=EDGE_CURVE('',#1629,#1626,#838,.T.);
#1991=EDGE_CURVE('',#1635,#1636,#839,.T.);
#1992=EDGE_CURVE('',#1635,#1637,#1055,.T.);
#1993=EDGE_CURVE('',#1638,#1637,#840,.T.);
#1994=EDGE_CURVE('',#1636,#1638,#1056,.T.);
#1995=EDGE_CURVE('',#1636,#1639,#1057,.T.);
#1996=EDGE_CURVE('',#1640,#1638,#1058,.T.);
#1997=EDGE_CURVE('',#1639,#1640,#1059,.T.);
#1998=EDGE_CURVE('',#1641,#1635,#1060,.T.);
#1999=EDGE_CURVE('',#1641,#1642,#1061,.T.);
#2000=EDGE_CURVE('',#1637,#1642,#1062,.T.);
#2001=EDGE_CURVE('',#1643,#1643,#841,.T.);
#2002=EDGE_CURVE('',#1643,#1644,#1063,.T.);
#2003=EDGE_CURVE('',#1641,#1644,#842,.T.);
#2004=EDGE_CURVE('',#1644,#1639,#843,.T.);
#2005=EDGE_CURVE('',#1645,#1645,#844,.T.);
#2006=EDGE_CURVE('',#1645,#1646,#1064,.T.);
#2007=EDGE_CURVE('',#1646,#1646,#845,.T.);
#2008=EDGE_CURVE('',#1642,#1640,#846,.T.);
#2009=EDGE_CURVE('',#1647,#1647,#847,.T.);
#2010=EDGE_CURVE('',#1647,#1648,#1065,.T.);
#2011=EDGE_CURVE('',#1648,#1648,#848,.T.);
#2012=EDGE_CURVE('',#1649,#1649,#849,.T.);
#2013=EDGE_CURVE('',#1649,#1650,#1066,.T.);
#2014=EDGE_CURVE('',#1650,#1650,#850,.T.);
#2015=EDGE_CURVE('',#1651,#1651,#851,.T.);
#2016=EDGE_CURVE('',#1651,#1652,#1067,.T.);
#2017=EDGE_CURVE('',#1652,#1652,#852,.T.);
#2018=EDGE_CURVE('',#1653,#1653,#853,.T.);
#2019=EDGE_CURVE('',#1653,#1654,#1068,.T.);
#2020=EDGE_CURVE('',#1654,#1654,#854,.T.);
#2021=EDGE_CURVE('',#1655,#1655,#855,.T.);
#2022=EDGE_CURVE('',#1655,#1656,#1069,.T.);
#2023=EDGE_CURVE('',#1656,#1656,#856,.T.);
#2024=EDGE_CURVE('',#1657,#1657,#857,.T.);
#2025=EDGE_CURVE('',#1657,#1658,#1070,.T.);
#2026=EDGE_CURVE('',#1658,#1658,#858,.T.);
#2027=EDGE_CURVE('',#1659,#1659,#859,.T.);
#2028=EDGE_CURVE('',#1659,#1660,#1071,.T.);
#2029=EDGE_CURVE('',#1660,#1660,#860,.T.);
#2030=EDGE_CURVE('',#1661,#1661,#861,.T.);
#2031=EDGE_CURVE('',#1661,#1662,#1072,.T.);
#2032=EDGE_CURVE('',#1662,#1662,#862,.T.);
#2033=EDGE_CURVE('',#1663,#1663,#863,.T.);
#2034=EDGE_CURVE('',#1663,#1664,#1073,.T.);
#2035=EDGE_CURVE('',#1664,#1664,#864,.T.);
#2036=EDGE_CURVE('',#1665,#1665,#865,.T.);
#2037=EDGE_CURVE('',#1665,#1666,#1074,.T.);
#2038=EDGE_CURVE('',#1666,#1666,#866,.T.);
#2039=EDGE_CURVE('',#1667,#1667,#867,.T.);
#2040=EDGE_CURVE('',#1667,#1668,#1075,.T.);
#2041=EDGE_CURVE('',#1668,#1668,#868,.T.);
#2042=EDGE_CURVE('',#1669,#1669,#869,.T.);
#2043=EDGE_CURVE('',#1669,#1670,#1076,.T.);
#2044=EDGE_CURVE('',#1670,#1670,#870,.T.);
#2045=EDGE_CURVE('',#1671,#1671,#871,.T.);
#2046=EDGE_CURVE('',#1671,#1672,#1077,.T.);
#2047=EDGE_CURVE('',#1672,#1672,#872,.T.);
#2048=EDGE_CURVE('',#1673,#1673,#873,.T.);
#2049=EDGE_CURVE('',#1673,#1674,#1078,.T.);
#2050=EDGE_CURVE('',#1674,#1674,#874,.T.);
#2051=EDGE_CURVE('',#1675,#1675,#875,.T.);
#2052=EDGE_CURVE('',#1675,#1676,#1079,.T.);
#2053=EDGE_CURVE('',#1676,#1676,#876,.T.);
#2054=EDGE_CURVE('',#1677,#1677,#877,.T.);
#2055=EDGE_CURVE('',#1677,#1678,#1080,.T.);
#2056=EDGE_CURVE('',#1678,#1678,#878,.T.);
#2057=EDGE_CURVE('',#1679,#1679,#879,.T.);
#2058=EDGE_CURVE('',#1679,#1680,#1081,.T.);
#2059=EDGE_CURVE('',#1680,#1680,#880,.T.);
#2060=EDGE_CURVE('',#1681,#1682,#70,.T.);
#2061=EDGE_CURVE('',#1683,#1681,#881,.T.);
#2062=EDGE_CURVE('',#1684,#1683,#71,.T.);
#2063=EDGE_CURVE('',#1682,#1684,#882,.T.);
#2064=EDGE_CURVE('',#1685,#1686,#65,.T.);
#2065=EDGE_CURVE('',#1686,#1687,#883,.T.);
#2066=EDGE_CURVE('',#1687,#1688,#66,.T.);
#2067=EDGE_CURVE('',#1688,#1683,#67,.T.);
#2068=EDGE_CURVE('',#1681,#1685,#68,.T.);
#2069=EDGE_CURVE('',#1689,#1686,#72,.T.);
#2070=EDGE_CURVE('',#1690,#1689,#884,.T.);
#2071=EDGE_CURVE('',#1687,#1690,#73,.T.);
#2072=EDGE_CURVE('',#1690,#1689,#885,.T.);
#2073=EDGE_CURVE('',#1682,#1684,#886,.T.);
#2074=EDGE_CURVE('',#1691,#1691,#887,.T.);
#2075=EDGE_CURVE('',#1691,#1692,#1082,.T.);
#2076=EDGE_CURVE('',#1692,#1693,#888,.T.);
#2077=EDGE_CURVE('',#1693,#1692,#889,.T.);
#2078=EDGE_CURVE('',#1693,#1694,#1083,.T.);
#2079=EDGE_CURVE('',#1694,#1694,#890,.T.);
#2080=EDGE_CURVE('',#1694,#1685,#1084,.T.);
#2081=EDGE_CURVE('',#1695,#1695,#69,.T.);
#2082=EDGE_CURVE('',#1695,#1696,#1085,.T.);
#2083=EDGE_CURVE('',#1696,#1696,#891,.T.);
#2084=EDGE_CURVE('',#1697,#1698,#1086,.T.);
#2085=EDGE_CURVE('',#1699,#1697,#1087,.T.);
#2086=EDGE_CURVE('',#1700,#1699,#1088,.T.);
#2087=EDGE_CURVE('',#1698,#1700,#1089,.T.);
#2088=EDGE_CURVE('',#1701,#1702,#1090,.T.);
#2089=EDGE_CURVE('',#1703,#1701,#1091,.T.);
#2090=EDGE_CURVE('',#1704,#1703,#1092,.T.);
#2091=EDGE_CURVE('',#1702,#1704,#1093,.T.);
#2092=EDGE_CURVE('',#1705,#1706,#1094,.T.);
#2093=EDGE_CURVE('',#1707,#1705,#1095,.T.);
#2094=EDGE_CURVE('',#1708,#1707,#1096,.T.);
#2095=EDGE_CURVE('',#1706,#1708,#1097,.T.);
#2096=EDGE_CURVE('',#1709,#1710,#1098,.T.);
#2097=EDGE_CURVE('',#1711,#1709,#1099,.T.);
#2098=EDGE_CURVE('',#1712,#1711,#1100,.T.);
#2099=EDGE_CURVE('',#1710,#1712,#1101,.T.);
#2100=EDGE_CURVE('',#1713,#1714,#1102,.T.);
#2101=EDGE_CURVE('',#1715,#1713,#1103,.T.);
#2102=EDGE_CURVE('',#1716,#1715,#1104,.T.);
#2103=EDGE_CURVE('',#1714,#1716,#1105,.T.);
#2104=EDGE_CURVE('',#1717,#1718,#1106,.T.);
#2105=EDGE_CURVE('',#1719,#1717,#1107,.T.);
#2106=EDGE_CURVE('',#1720,#1719,#1108,.T.);
#2107=EDGE_CURVE('',#1718,#1720,#1109,.T.);
#2108=EDGE_CURVE('',#1721,#1722,#1110,.T.);
#2109=EDGE_CURVE('',#1723,#1721,#1111,.T.);
#2110=EDGE_CURVE('',#1724,#1723,#1112,.T.);
#2111=EDGE_CURVE('',#1722,#1724,#1113,.T.);
#2112=EDGE_CURVE('',#1725,#1726,#1114,.T.);
#2113=EDGE_CURVE('',#1727,#1725,#1115,.T.);
#2114=EDGE_CURVE('',#1728,#1727,#1116,.T.);
#2115=EDGE_CURVE('',#1726,#1728,#1117,.T.);
#2116=EDGE_CURVE('',#1729,#1730,#1118,.T.);
#2117=EDGE_CURVE('',#1731,#1729,#1119,.T.);
#2118=EDGE_CURVE('',#1732,#1731,#1120,.T.);
#2119=EDGE_CURVE('',#1730,#1732,#1121,.T.);
#2120=EDGE_CURVE('',#1733,#1734,#1122,.T.);
#2121=EDGE_CURVE('',#1735,#1733,#1123,.T.);
#2122=EDGE_CURVE('',#1736,#1735,#1124,.T.);
#2123=EDGE_CURVE('',#1734,#1736,#1125,.T.);
#2124=EDGE_CURVE('',#1737,#1738,#1126,.T.);
#2125=EDGE_CURVE('',#1739,#1737,#1127,.T.);
#2126=EDGE_CURVE('',#1740,#1739,#1128,.T.);
#2127=EDGE_CURVE('',#1738,#1740,#1129,.T.);
#2128=EDGE_CURVE('',#1741,#1742,#1130,.T.);
#2129=EDGE_CURVE('',#1743,#1741,#1131,.T.);
#2130=EDGE_CURVE('',#1744,#1743,#1132,.T.);
#2131=EDGE_CURVE('',#1742,#1744,#1133,.T.);
#2132=EDGE_CURVE('',#1745,#1746,#1134,.T.);
#2133=EDGE_CURVE('',#1747,#1745,#1135,.T.);
#2134=EDGE_CURVE('',#1748,#1747,#1136,.T.);
#2135=EDGE_CURVE('',#1746,#1748,#1137,.T.);
#2136=EDGE_CURVE('',#1749,#1750,#1138,.T.);
#2137=EDGE_CURVE('',#1751,#1749,#1139,.T.);
#2138=EDGE_CURVE('',#1752,#1751,#1140,.T.);
#2139=EDGE_CURVE('',#1750,#1752,#1141,.T.);
#2140=EDGE_CURVE('',#1753,#1754,#1142,.T.);
#2141=EDGE_CURVE('',#1755,#1753,#1143,.T.);
#2142=EDGE_CURVE('',#1756,#1755,#1144,.T.);
#2143=EDGE_CURVE('',#1754,#1756,#1145,.T.);
#2144=EDGE_CURVE('',#1757,#1758,#1146,.T.);
#2145=EDGE_CURVE('',#1759,#1757,#1147,.T.);
#2146=EDGE_CURVE('',#1760,#1759,#1148,.T.);
#2147=EDGE_CURVE('',#1758,#1760,#1149,.T.);
#2148=EDGE_CURVE('',#1761,#1762,#1150,.T.);
#2149=EDGE_CURVE('',#1763,#1761,#1151,.T.);
#2150=EDGE_CURVE('',#1764,#1763,#1152,.T.);
#2151=EDGE_CURVE('',#1762,#1764,#1153,.T.);
#2152=EDGE_CURVE('',#1765,#1766,#1154,.T.);
#2153=EDGE_CURVE('',#1767,#1765,#1155,.T.);
#2154=EDGE_CURVE('',#1768,#1767,#1156,.T.);
#2155=EDGE_CURVE('',#1766,#1768,#1157,.T.);
#2156=EDGE_CURVE('',#1769,#1770,#1158,.T.);
#2157=EDGE_CURVE('',#1771,#1769,#1159,.T.);
#2158=EDGE_CURVE('',#1772,#1771,#1160,.T.);
#2159=EDGE_CURVE('',#1770,#1772,#1161,.T.);
#2160=EDGE_CURVE('',#1773,#1774,#892,.T.);
#2161=EDGE_CURVE('',#1773,#1775,#1162,.T.);
#2162=EDGE_CURVE('',#1776,#1775,#893,.T.);
#2163=EDGE_CURVE('',#1771,#1776,#894,.T.);
#2164=EDGE_CURVE('',#1774,#1769,#895,.T.);
#2165=EDGE_CURVE('',#1777,#1765,#896,.T.);
#2166=EDGE_CURVE('',#1777,#1778,#1163,.T.);
#2167=EDGE_CURVE('',#1767,#1778,#897,.T.);
#2168=EDGE_CURVE('',#1779,#1761,#898,.T.);
#2169=EDGE_CURVE('',#1779,#1780,#1164,.T.);
#2170=EDGE_CURVE('',#1763,#1780,#899,.T.);
#2171=EDGE_CURVE('',#1781,#1757,#900,.T.);
#2172=EDGE_CURVE('',#1781,#1782,#1165,.T.);
#2173=EDGE_CURVE('',#1759,#1782,#901,.T.);
#2174=EDGE_CURVE('',#1783,#1753,#902,.T.);
#2175=EDGE_CURVE('',#1783,#1784,#1166,.T.);
#2176=EDGE_CURVE('',#1755,#1784,#903,.T.);
#2177=EDGE_CURVE('',#1785,#1749,#904,.T.);
#2178=EDGE_CURVE('',#1785,#1786,#1167,.T.);
#2179=EDGE_CURVE('',#1751,#1786,#905,.T.);
#2180=EDGE_CURVE('',#1787,#1745,#906,.T.);
#2181=EDGE_CURVE('',#1787,#1788,#1168,.T.);
#2182=EDGE_CURVE('',#1747,#1788,#907,.T.);
#2183=EDGE_CURVE('',#1789,#1741,#908,.T.);
#2184=EDGE_CURVE('',#1789,#1790,#1169,.T.);
#2185=EDGE_CURVE('',#1743,#1790,#909,.T.);
#2186=EDGE_CURVE('',#1791,#1737,#910,.T.);
#2187=EDGE_CURVE('',#1791,#1792,#1170,.T.);
#2188=EDGE_CURVE('',#1739,#1792,#911,.T.);
#2189=EDGE_CURVE('',#1793,#1733,#912,.T.);
#2190=EDGE_CURVE('',#1793,#1794,#1171,.T.);
#2191=EDGE_CURVE('',#1735,#1794,#913,.T.);
#2192=EDGE_CURVE('',#1795,#1729,#914,.T.);
#2193=EDGE_CURVE('',#1795,#1796,#1172,.T.);
#2194=EDGE_CURVE('',#1731,#1796,#915,.T.);
#2195=EDGE_CURVE('',#1797,#1725,#916,.T.);
#2196=EDGE_CURVE('',#1797,#1798,#1173,.T.);
#2197=EDGE_CURVE('',#1727,#1798,#917,.T.);
#2198=EDGE_CURVE('',#1799,#1721,#918,.T.);
#2199=EDGE_CURVE('',#1799,#1800,#1174,.T.);
#2200=EDGE_CURVE('',#1723,#1800,#919,.T.);
#2201=EDGE_CURVE('',#1801,#1717,#920,.T.);
#2202=EDGE_CURVE('',#1801,#1802,#1175,.T.);
#2203=EDGE_CURVE('',#1719,#1802,#921,.T.);
#2204=EDGE_CURVE('',#1803,#1713,#922,.T.);
#2205=EDGE_CURVE('',#1803,#1804,#1176,.T.);
#2206=EDGE_CURVE('',#1715,#1804,#923,.T.);
#2207=EDGE_CURVE('',#1805,#1709,#924,.T.);
#2208=EDGE_CURVE('',#1805,#1806,#1177,.T.);
#2209=EDGE_CURVE('',#1711,#1806,#925,.T.);
#2210=EDGE_CURVE('',#1807,#1705,#926,.T.);
#2211=EDGE_CURVE('',#1807,#1808,#1178,.T.);
#2212=EDGE_CURVE('',#1707,#1808,#927,.T.);
#2213=EDGE_CURVE('',#1809,#1701,#928,.T.);
#2214=EDGE_CURVE('',#1809,#1810,#1179,.T.);
#2215=EDGE_CURVE('',#1703,#1810,#929,.T.);
#2216=EDGE_CURVE('',#1811,#1697,#930,.T.);
#2217=EDGE_CURVE('',#1811,#1812,#1180,.T.);
#2218=EDGE_CURVE('',#1699,#1812,#931,.T.);
#2219=EDGE_CURVE('',#1813,#1785,#1181,.T.);
#2220=EDGE_CURVE('',#1814,#1813,#1182,.T.);
#2221=EDGE_CURVE('',#1786,#1814,#1183,.T.);
#2222=EDGE_CURVE('',#1815,#1801,#1184,.T.);
#2223=EDGE_CURVE('',#1816,#1815,#1185,.T.);
#2224=EDGE_CURVE('',#1802,#1816,#1186,.T.);
#2225=EDGE_CURVE('',#1817,#1803,#1187,.T.);
#2226=EDGE_CURVE('',#1818,#1817,#1188,.T.);
#2227=EDGE_CURVE('',#1804,#1818,#1189,.T.);
#2228=EDGE_CURVE('',#1819,#1783,#1190,.T.);
#2229=EDGE_CURVE('',#1820,#1819,#1191,.T.);
#2230=EDGE_CURVE('',#1784,#1820,#1192,.T.);
#2231=EDGE_CURVE('',#1821,#1811,#1193,.T.);
#2232=EDGE_CURVE('',#1822,#1821,#1194,.T.);
#2233=EDGE_CURVE('',#1812,#1822,#1195,.T.);
#2234=EDGE_CURVE('',#1823,#1799,#1196,.T.);
#2235=EDGE_CURVE('',#1824,#1823,#1197,.T.);
#2236=EDGE_CURVE('',#1800,#1824,#1198,.T.);
#2237=EDGE_CURVE('',#1825,#1781,#1199,.T.);
#2238=EDGE_CURVE('',#1826,#1825,#1200,.T.);
#2239=EDGE_CURVE('',#1782,#1826,#1201,.T.);
#2240=EDGE_CURVE('',#1827,#1779,#1202,.T.);
#2241=EDGE_CURVE('',#1828,#1827,#1203,.T.);
#2242=EDGE_CURVE('',#1780,#1828,#1204,.T.);
#2243=EDGE_CURVE('',#1829,#1797,#1205,.T.);
#2244=EDGE_CURVE('',#1830,#1829,#1206,.T.);
#2245=EDGE_CURVE('',#1798,#1830,#1207,.T.);
#2246=EDGE_CURVE('',#1831,#1795,#1208,.T.);
#2247=EDGE_CURVE('',#1832,#1831,#1209,.T.);
#2248=EDGE_CURVE('',#1796,#1832,#1210,.T.);
#2249=EDGE_CURVE('',#1833,#1777,#1211,.T.);
#2250=EDGE_CURVE('',#1834,#1833,#1212,.T.);
#2251=EDGE_CURVE('',#1778,#1834,#1213,.T.);
#2252=EDGE_CURVE('',#1835,#1773,#1214,.T.);
#2253=EDGE_CURVE('',#1836,#1835,#1215,.T.);
#2254=EDGE_CURVE('',#1775,#1836,#1216,.T.);
#2255=EDGE_CURVE('',#1837,#1793,#1217,.T.);
#2256=EDGE_CURVE('',#1838,#1837,#1218,.T.);
#2257=EDGE_CURVE('',#1794,#1838,#1219,.T.);
#2258=EDGE_CURVE('',#1839,#1791,#1220,.T.);
#2259=EDGE_CURVE('',#1840,#1839,#1221,.T.);
#2260=EDGE_CURVE('',#1792,#1840,#1222,.T.);
#2261=EDGE_CURVE('',#1841,#1809,#1223,.T.);
#2262=EDGE_CURVE('',#1842,#1841,#1224,.T.);
#2263=EDGE_CURVE('',#1810,#1842,#1225,.T.);
#2264=EDGE_CURVE('',#1843,#1807,#1226,.T.);
#2265=EDGE_CURVE('',#1844,#1843,#1227,.T.);
#2266=EDGE_CURVE('',#1808,#1844,#1228,.T.);
#2267=EDGE_CURVE('',#1845,#1789,#1229,.T.);
#2268=EDGE_CURVE('',#1846,#1845,#1230,.T.);
#2269=EDGE_CURVE('',#1790,#1846,#1231,.T.);
#2270=EDGE_CURVE('',#1847,#1805,#1232,.T.);
#2271=EDGE_CURVE('',#1848,#1847,#1233,.T.);
#2272=EDGE_CURVE('',#1806,#1848,#1234,.T.);
#2273=EDGE_CURVE('',#1849,#1787,#1235,.T.);
#2274=EDGE_CURVE('',#1850,#1849,#1236,.T.);
#2275=EDGE_CURVE('',#1788,#1850,#1237,.T.);
#2276=EDGE_CURVE('',#1851,#1851,#932,.T.);
#2277=EDGE_CURVE('',#1851,#1774,#1238,.T.);
#2278=EDGE_CURVE('',#1770,#1833,#933,.T.);
#2279=EDGE_CURVE('',#1766,#1827,#934,.T.);
#2280=EDGE_CURVE('',#1762,#1825,#935,.T.);
#2281=EDGE_CURVE('',#1758,#1819,#936,.T.);
#2282=EDGE_CURVE('',#1754,#1852,#937,.T.);
#2283=EDGE_CURVE('',#1852,#1853,#1239,.T.);
#2284=EDGE_CURVE('',#1853,#1854,#938,.T.);
#2285=EDGE_CURVE('',#1854,#1855,#1240,.T.);
#2286=EDGE_CURVE('',#1855,#1813,#939,.T.);
#2287=EDGE_CURVE('',#1750,#1849,#940,.T.);
#2288=EDGE_CURVE('',#1746,#1845,#941,.T.);
#2289=EDGE_CURVE('',#1742,#1839,#942,.T.);
#2290=EDGE_CURVE('',#1738,#1837,#943,.T.);
#2291=EDGE_CURVE('',#1734,#1831,#944,.T.);
#2292=EDGE_CURVE('',#1730,#1829,#945,.T.);
#2293=EDGE_CURVE('',#1726,#1823,#946,.T.);
#2294=EDGE_CURVE('',#1722,#1821,#947,.T.);
#2295=EDGE_CURVE('',#1698,#1815,#948,.T.);
#2296=EDGE_CURVE('',#1718,#1817,#949,.T.);
#2297=EDGE_CURVE('',#1714,#1847,#950,.T.);
#2298=EDGE_CURVE('',#1710,#1843,#951,.T.);
#2299=EDGE_CURVE('',#1706,#1841,#952,.T.);
#2300=EDGE_CURVE('',#1702,#1835,#953,.T.);
#2301=EDGE_CURVE('',#1856,#1756,#954,.T.);
#2302=EDGE_CURVE('',#1856,#1852,#1241,.T.);
#2303=EDGE_CURVE('',#1836,#1704,#955,.T.);
#2304=EDGE_CURVE('',#1834,#1772,#956,.T.);
#2305=EDGE_CURVE('',#1828,#1768,#957,.T.);
#2306=EDGE_CURVE('',#1826,#1764,#958,.T.);
#2307=EDGE_CURVE('',#1820,#1760,#959,.T.);
#2308=EDGE_CURVE('',#1855,#1857,#1242,.T.);
#2309=EDGE_CURVE('',#1814,#1857,#960,.T.);
#2310=EDGE_CURVE('',#1850,#1752,#961,.T.);
#2311=EDGE_CURVE('',#1846,#1748,#962,.T.);
#2312=EDGE_CURVE('',#1840,#1744,#963,.T.);
#2313=EDGE_CURVE('',#1838,#1740,#964,.T.);
#2314=EDGE_CURVE('',#1832,#1736,#965,.T.);
#2315=EDGE_CURVE('',#1830,#1732,#966,.T.);
#2316=EDGE_CURVE('',#1824,#1728,#967,.T.);
#2317=EDGE_CURVE('',#1816,#1700,#968,.T.);
#2318=EDGE_CURVE('',#1818,#1720,#969,.T.);
#2319=EDGE_CURVE('',#1848,#1716,#970,.T.);
#2320=EDGE_CURVE('',#1844,#1712,#971,.T.);
#2321=EDGE_CURVE('',#1842,#1708,#972,.T.);
#2322=EDGE_CURVE('',#1858,#1854,#1243,.T.);
#2323=EDGE_CURVE('',#1857,#1858,#1244,.T.);
#2324=EDGE_CURVE('',#1853,#1859,#1245,.T.);
#2325=EDGE_CURVE('',#1858,#1859,#973,.T.);
#2326=EDGE_CURVE('',#1859,#1856,#1246,.T.);
#2327=EDGE_CURVE('',#1860,#1860,#974,.T.);
#2328=EDGE_CURVE('',#1860,#1776,#1247,.T.);
#2329=EDGE_CURVE('',#1822,#1724,#975,.T.);
#2330=EDGE_CURVE('',#1861,#1862,#1248,.T.);
#2331=EDGE_CURVE('',#1863,#1861,#1249,.T.);
#2332=EDGE_CURVE('',#1864,#1863,#1250,.T.);
#2333=EDGE_CURVE('',#1862,#1864,#1251,.T.);
#2334=EDGE_CURVE('',#1865,#1866,#1252,.T.);
#2335=EDGE_CURVE('',#1867,#1865,#1253,.T.);
#2336=EDGE_CURVE('',#1868,#1867,#1254,.T.);
#2337=EDGE_CURVE('',#1866,#1868,#1255,.T.);
#2338=EDGE_CURVE('',#1865,#1862,#976,.T.);
#2339=EDGE_CURVE('',#1861,#1866,#977,.T.);
#2340=EDGE_CURVE('',#1869,#1869,#978,.T.);
#2341=EDGE_CURVE('',#1870,#1870,#979,.T.);
#2342=EDGE_CURVE('',#1871,#1871,#980,.T.);
#2343=EDGE_CURVE('',#1871,#1869,#1256,.T.);
#2344=EDGE_CURVE('',#1872,#1872,#981,.T.);
#2345=EDGE_CURVE('',#1872,#1870,#1257,.T.);
#2346=EDGE_CURVE('',#1863,#1868,#982,.T.);
#2347=EDGE_CURVE('',#1867,#1864,#983,.T.);
#2348=EDGE_CURVE('',#1873,#1874,#1258,.T.);
#2349=EDGE_CURVE('',#1875,#1873,#1259,.T.);
#2350=EDGE_CURVE('',#1876,#1875,#1260,.T.);
#2351=EDGE_CURVE('',#1874,#1876,#1261,.T.);
#2352=EDGE_CURVE('',#1877,#1878,#1262,.T.);
#2353=EDGE_CURVE('',#1879,#1877,#1263,.T.);
#2354=EDGE_CURVE('',#1880,#1879,#1264,.T.);
#2355=EDGE_CURVE('',#1878,#1880,#1265,.T.);
#2356=EDGE_CURVE('',#1877,#1874,#984,.T.);
#2357=EDGE_CURVE('',#1873,#1878,#985,.T.);
#2358=EDGE_CURVE('',#1881,#1881,#986,.T.);
#2359=EDGE_CURVE('',#1882,#1882,#987,.T.);
#2360=EDGE_CURVE('',#1883,#1883,#988,.T.);
#2361=EDGE_CURVE('',#1883,#1881,#1266,.T.);
#2362=EDGE_CURVE('',#1884,#1884,#989,.T.);
#2363=EDGE_CURVE('',#1884,#1882,#1267,.T.);
#2364=EDGE_CURVE('',#1875,#1880,#990,.T.);
#2365=EDGE_CURVE('',#1879,#1876,#991,.T.);
#2366=EDGE_CURVE('',#1885,#1886,#1268,.T.);
#2367=EDGE_CURVE('',#1887,#1885,#1269,.T.);
#2368=EDGE_CURVE('',#1888,#1887,#1270,.T.);
#2369=EDGE_CURVE('',#1886,#1888,#1271,.T.);
#2370=EDGE_CURVE('',#1889,#1890,#1272,.T.);
#2371=EDGE_CURVE('',#1891,#1889,#1273,.T.);
#2372=EDGE_CURVE('',#1892,#1891,#1274,.T.);
#2373=EDGE_CURVE('',#1890,#1892,#1275,.T.);
#2374=EDGE_CURVE('',#1889,#1886,#992,.T.);
#2375=EDGE_CURVE('',#1885,#1890,#993,.T.);
#2376=EDGE_CURVE('',#1893,#1893,#994,.T.);
#2377=EDGE_CURVE('',#1894,#1894,#995,.T.);
#2378=EDGE_CURVE('',#1895,#1895,#996,.T.);
#2379=EDGE_CURVE('',#1895,#1893,#1276,.T.);
#2380=EDGE_CURVE('',#1896,#1896,#997,.T.);
#2381=EDGE_CURVE('',#1896,#1894,#1277,.T.);
#2382=EDGE_CURVE('',#1887,#1892,#998,.T.);
#2383=EDGE_CURVE('',#1891,#1888,#999,.T.);
#2384=EDGE_CURVE('',#1897,#1898,#1278,.T.);
#2385=EDGE_CURVE('',#1899,#1897,#1279,.T.);
#2386=EDGE_CURVE('',#1900,#1899,#1280,.T.);
#2387=EDGE_CURVE('',#1898,#1900,#1281,.T.);
#2388=EDGE_CURVE('',#1901,#1902,#1282,.T.);
#2389=EDGE_CURVE('',#1903,#1901,#1283,.T.);
#2390=EDGE_CURVE('',#1904,#1903,#1284,.T.);
#2391=EDGE_CURVE('',#1902,#1904,#1285,.T.);
#2392=EDGE_CURVE('',#1901,#1898,#1000,.T.);
#2393=EDGE_CURVE('',#1897,#1902,#1001,.T.);
#2394=EDGE_CURVE('',#1905,#1905,#1002,.T.);
#2395=EDGE_CURVE('',#1906,#1906,#1003,.T.);
#2396=EDGE_CURVE('',#1907,#1907,#1004,.T.);
#2397=EDGE_CURVE('',#1907,#1905,#1286,.T.);
#2398=EDGE_CURVE('',#1908,#1908,#1005,.T.);
#2399=EDGE_CURVE('',#1908,#1906,#1287,.T.);
#2400=EDGE_CURVE('',#1899,#1904,#1006,.T.);
#2401=EDGE_CURVE('',#1903,#1900,#1007,.T.);
#2402=EDGE_CURVE('',#1909,#1910,#1288,.T.);
#2403=EDGE_CURVE('',#1911,#1909,#1289,.T.);
#2404=EDGE_CURVE('',#1912,#1911,#1290,.T.);
#2405=EDGE_CURVE('',#1910,#1912,#1291,.T.);
#2406=EDGE_CURVE('',#1913,#1914,#1292,.T.);
#2407=EDGE_CURVE('',#1915,#1913,#1293,.T.);
#2408=EDGE_CURVE('',#1916,#1915,#1294,.T.);
#2409=EDGE_CURVE('',#1914,#1916,#1295,.T.);
#2410=EDGE_CURVE('',#1913,#1910,#1008,.T.);
#2411=EDGE_CURVE('',#1909,#1914,#1009,.T.);
#2412=EDGE_CURVE('',#1917,#1917,#1010,.T.);
#2413=EDGE_CURVE('',#1918,#1918,#1011,.T.);
#2414=EDGE_CURVE('',#1919,#1919,#1012,.T.);
#2415=EDGE_CURVE('',#1919,#1917,#1296,.T.);
#2416=EDGE_CURVE('',#1920,#1920,#1013,.T.);
#2417=EDGE_CURVE('',#1920,#1918,#1297,.T.);
#2418=EDGE_CURVE('',#1911,#1916,#1014,.T.);
#2419=EDGE_CURVE('',#1915,#1912,#1015,.T.);
#2420=EDGE_CURVE('',#1921,#1922,#1298,.T.);
#2421=EDGE_CURVE('',#1923,#1921,#1299,.T.);
#2422=EDGE_CURVE('',#1924,#1923,#1300,.T.);
#2423=EDGE_CURVE('',#1922,#1924,#1301,.T.);
#2424=EDGE_CURVE('',#1925,#1926,#1302,.T.);
#2425=EDGE_CURVE('',#1927,#1925,#1303,.T.);
#2426=EDGE_CURVE('',#1928,#1927,#1304,.T.);
#2427=EDGE_CURVE('',#1926,#1928,#1305,.T.);
#2428=EDGE_CURVE('',#1925,#1922,#1016,.T.);
#2429=EDGE_CURVE('',#1921,#1926,#1017,.T.);
#2430=EDGE_CURVE('',#1929,#1929,#1018,.T.);
#2431=EDGE_CURVE('',#1930,#1930,#1019,.T.);
#2432=EDGE_CURVE('',#1931,#1931,#1020,.T.);
#2433=EDGE_CURVE('',#1931,#1929,#1306,.T.);
#2434=EDGE_CURVE('',#1932,#1932,#1021,.T.);
#2435=EDGE_CURVE('',#1932,#1930,#1307,.T.);
#2436=EDGE_CURVE('',#1923,#1928,#1022,.T.);
#2437=EDGE_CURVE('',#1927,#1924,#1023,.T.);
#2438=EDGE_CURVE('',#1933,#1934,#1308,.T.);
#2439=EDGE_CURVE('',#1935,#1933,#1309,.T.);
#2440=EDGE_CURVE('',#1936,#1935,#1310,.T.);
#2441=EDGE_CURVE('',#1934,#1936,#1311,.T.);
#2442=EDGE_CURVE('',#1937,#1938,#1312,.T.);
#2443=EDGE_CURVE('',#1939,#1937,#1313,.T.);
#2444=EDGE_CURVE('',#1940,#1939,#1314,.T.);
#2445=EDGE_CURVE('',#1938,#1940,#1315,.T.);
#2446=EDGE_CURVE('',#1937,#1934,#1024,.T.);
#2447=EDGE_CURVE('',#1933,#1938,#1025,.T.);
#2448=EDGE_CURVE('',#1941,#1941,#1026,.T.);
#2449=EDGE_CURVE('',#1942,#1942,#1027,.T.);
#2450=EDGE_CURVE('',#1943,#1943,#1028,.T.);
#2451=EDGE_CURVE('',#1943,#1941,#1316,.T.);
#2452=EDGE_CURVE('',#1944,#1944,#1029,.T.);
#2453=EDGE_CURVE('',#1944,#1942,#1317,.T.);
#2454=EDGE_CURVE('',#1935,#1940,#1030,.T.);
#2455=EDGE_CURVE('',#1939,#1936,#1031,.T.);
#2456=ORIENTED_EDGE('',*,*,#1945,.F.);
#2457=ORIENTED_EDGE('',*,*,#1946,.F.);
#2458=ORIENTED_EDGE('',*,*,#1947,.T.);
#2459=ORIENTED_EDGE('',*,*,#1948,.T.);
#2460=ORIENTED_EDGE('',*,*,#1947,.F.);
#2461=ORIENTED_EDGE('',*,*,#1949,.F.);
#2462=ORIENTED_EDGE('',*,*,#1950,.T.);
#2463=ORIENTED_EDGE('',*,*,#1951,.T.);
#2464=ORIENTED_EDGE('',*,*,#1948,.F.);
#2465=ORIENTED_EDGE('',*,*,#1952,.F.);
#2466=ORIENTED_EDGE('',*,*,#1949,.T.);
#2467=ORIENTED_EDGE('',*,*,#1946,.T.);
#2468=ORIENTED_EDGE('',*,*,#1953,.T.);
#2469=ORIENTED_EDGE('',*,*,#1954,.T.);
#2470=ORIENTED_EDGE('',*,*,#1955,.T.);
#2471=ORIENTED_EDGE('',*,*,#1956,.T.);
#2472=ORIENTED_EDGE('',*,*,#1956,.F.);
#2473=ORIENTED_EDGE('',*,*,#1957,.F.);
#2474=ORIENTED_EDGE('',*,*,#1958,.T.);
#2475=ORIENTED_EDGE('',*,*,#1950,.F.);
#2476=ORIENTED_EDGE('',*,*,#1953,.F.);
#2477=ORIENTED_EDGE('',*,*,#1945,.T.);
#2478=ORIENTED_EDGE('',*,*,#1959,.T.);
#2479=ORIENTED_EDGE('',*,*,#1960,.F.);
#2480=ORIENTED_EDGE('',*,*,#1961,.F.);
#2481=ORIENTED_EDGE('',*,*,#1959,.F.);
#2482=ORIENTED_EDGE('',*,*,#1951,.F.);
#2483=ORIENTED_EDGE('',*,*,#1958,.F.);
#2484=ORIENTED_EDGE('',*,*,#1962,.F.);
#2485=ORIENTED_EDGE('',*,*,#1963,.T.);
#2486=ORIENTED_EDGE('',*,*,#1952,.T.);
#2487=ORIENTED_EDGE('',*,*,#1963,.F.);
#2488=ORIENTED_EDGE('',*,*,#1964,.F.);
#2489=ORIENTED_EDGE('',*,*,#1965,.T.);
#2490=ORIENTED_EDGE('',*,*,#1954,.F.);
#2491=ORIENTED_EDGE('',*,*,#1960,.T.);
#2492=ORIENTED_EDGE('',*,*,#1961,.T.);
#2493=ORIENTED_EDGE('',*,*,#1957,.T.);
#2494=ORIENTED_EDGE('',*,*,#1955,.F.);
#2495=ORIENTED_EDGE('',*,*,#1965,.F.);
#2496=ORIENTED_EDGE('',*,*,#1964,.T.);
#2497=ORIENTED_EDGE('',*,*,#1962,.T.);
#2498=ORIENTED_EDGE('',*,*,#1966,.T.);
#2499=ORIENTED_EDGE('',*,*,#1967,.F.);
#2500=ORIENTED_EDGE('',*,*,#1967,.T.);
#2501=ORIENTED_EDGE('',*,*,#1966,.F.);
#2502=ORIENTED_EDGE('',*,*,#1968,.T.);
#2503=ORIENTED_EDGE('',*,*,#1969,.T.);
#2504=ORIENTED_EDGE('',*,*,#1968,.F.);
#2505=ORIENTED_EDGE('',*,*,#1969,.F.);
#2506=ORIENTED_EDGE('',*,*,#1970,.T.);
#2507=ORIENTED_EDGE('',*,*,#1971,.F.);
#2508=ORIENTED_EDGE('',*,*,#1972,.T.);
#2509=ORIENTED_EDGE('',*,*,#1970,.F.);
#2510=ORIENTED_EDGE('',*,*,#1972,.F.);
#2511=ORIENTED_EDGE('',*,*,#1971,.T.);
#2512=ORIENTED_EDGE('',*,*,#1973,.F.);
#2513=ORIENTED_EDGE('',*,*,#1974,.F.);
#2514=ORIENTED_EDGE('',*,*,#1975,.F.);
#2515=ORIENTED_EDGE('',*,*,#1976,.F.);
#2516=ORIENTED_EDGE('',*,*,#1977,.F.);
#2517=ORIENTED_EDGE('',*,*,#1978,.F.);
#2518=ORIENTED_EDGE('',*,*,#1979,.F.);
#2519=ORIENTED_EDGE('',*,*,#1980,.F.);
#2520=ORIENTED_EDGE('',*,*,#1973,.T.);
#2521=ORIENTED_EDGE('',*,*,#1981,.F.);
#2522=ORIENTED_EDGE('',*,*,#1977,.T.);
#2523=ORIENTED_EDGE('',*,*,#1982,.F.);
#2524=ORIENTED_EDGE('',*,*,#1983,.T.);
#2525=ORIENTED_EDGE('',*,*,#1984,.T.);
#2526=ORIENTED_EDGE('',*,*,#1985,.F.);
#2527=ORIENTED_EDGE('',*,*,#1986,.T.);
#2528=ORIENTED_EDGE('',*,*,#1983,.F.);
#2529=ORIENTED_EDGE('',*,*,#1986,.F.);
#2530=ORIENTED_EDGE('',*,*,#1985,.T.);
#2531=ORIENTED_EDGE('',*,*,#1987,.F.);
#2532=ORIENTED_EDGE('',*,*,#1988,.T.);
#2533=ORIENTED_EDGE('',*,*,#1984,.F.);
#2534=ORIENTED_EDGE('',*,*,#1988,.F.);
#2535=ORIENTED_EDGE('',*,*,#1987,.T.);
#2536=ORIENTED_EDGE('',*,*,#1974,.T.);
#2537=ORIENTED_EDGE('',*,*,#1982,.T.);
#2538=ORIENTED_EDGE('',*,*,#1980,.T.);
#2539=ORIENTED_EDGE('',*,*,#1989,.F.);
#2540=ORIENTED_EDGE('',*,*,#1976,.T.);
#2541=ORIENTED_EDGE('',*,*,#1990,.F.);
#2542=ORIENTED_EDGE('',*,*,#1978,.T.);
#2543=ORIENTED_EDGE('',*,*,#1981,.T.);
#2544=ORIENTED_EDGE('',*,*,#1975,.T.);
#2545=ORIENTED_EDGE('',*,*,#1989,.T.);
#2546=ORIENTED_EDGE('',*,*,#1979,.T.);
#2547=ORIENTED_EDGE('',*,*,#1990,.T.);
#2548=ORIENTED_EDGE('',*,*,#1991,.F.);
#2549=ORIENTED_EDGE('',*,*,#1992,.T.);
#2550=ORIENTED_EDGE('',*,*,#1993,.F.);
#2551=ORIENTED_EDGE('',*,*,#1994,.F.);
#2552=ORIENTED_EDGE('',*,*,#1995,.F.);
#2553=ORIENTED_EDGE('',*,*,#1994,.T.);
#2554=ORIENTED_EDGE('',*,*,#1996,.F.);
#2555=ORIENTED_EDGE('',*,*,#1997,.F.);
#2556=ORIENTED_EDGE('',*,*,#1998,.F.);
#2557=ORIENTED_EDGE('',*,*,#1999,.T.);
#2558=ORIENTED_EDGE('',*,*,#2000,.F.);
#2559=ORIENTED_EDGE('',*,*,#1992,.F.);
#2560=ORIENTED_EDGE('',*,*,#2001,.F.);
#2561=ORIENTED_EDGE('',*,*,#2002,.T.);
#2562=ORIENTED_EDGE('',*,*,#2003,.F.);
#2563=ORIENTED_EDGE('',*,*,#1998,.T.);
#2564=ORIENTED_EDGE('',*,*,#1991,.T.);
#2565=ORIENTED_EDGE('',*,*,#1995,.T.);
#2566=ORIENTED_EDGE('',*,*,#2004,.F.);
#2567=ORIENTED_EDGE('',*,*,#2002,.F.);
#2568=ORIENTED_EDGE('',*,*,#2005,.F.);
#2569=ORIENTED_EDGE('',*,*,#2006,.T.);
#2570=ORIENTED_EDGE('',*,*,#2007,.F.);
#2571=ORIENTED_EDGE('',*,*,#2006,.F.);
#2572=ORIENTED_EDGE('',*,*,#2008,.T.);
#2573=ORIENTED_EDGE('',*,*,#1996,.T.);
#2574=ORIENTED_EDGE('',*,*,#1993,.T.);
#2575=ORIENTED_EDGE('',*,*,#2000,.T.);
#2576=ORIENTED_EDGE('',*,*,#2005,.T.);
#2577=ORIENTED_EDGE('',*,*,#2001,.T.);
#2578=ORIENTED_EDGE('',*,*,#2009,.F.);
#2579=ORIENTED_EDGE('',*,*,#2010,.T.);
#2580=ORIENTED_EDGE('',*,*,#2011,.F.);
#2581=ORIENTED_EDGE('',*,*,#2010,.F.);
#2582=ORIENTED_EDGE('',*,*,#2012,.F.);
#2583=ORIENTED_EDGE('',*,*,#2013,.T.);
#2584=ORIENTED_EDGE('',*,*,#2014,.F.);
#2585=ORIENTED_EDGE('',*,*,#2013,.F.);
#2586=ORIENTED_EDGE('',*,*,#2015,.F.);
#2587=ORIENTED_EDGE('',*,*,#2016,.T.);
#2588=ORIENTED_EDGE('',*,*,#2017,.F.);
#2589=ORIENTED_EDGE('',*,*,#2016,.F.);
#2590=ORIENTED_EDGE('',*,*,#2018,.F.);
#2591=ORIENTED_EDGE('',*,*,#2019,.T.);
#2592=ORIENTED_EDGE('',*,*,#2020,.F.);
#2593=ORIENTED_EDGE('',*,*,#2019,.F.);
#2594=ORIENTED_EDGE('',*,*,#2021,.F.);
#2595=ORIENTED_EDGE('',*,*,#2022,.T.);
#2596=ORIENTED_EDGE('',*,*,#2023,.F.);
#2597=ORIENTED_EDGE('',*,*,#2022,.F.);
#2598=ORIENTED_EDGE('',*,*,#2024,.F.);
#2599=ORIENTED_EDGE('',*,*,#2025,.T.);
#2600=ORIENTED_EDGE('',*,*,#2026,.F.);
#2601=ORIENTED_EDGE('',*,*,#2025,.F.);
#2602=ORIENTED_EDGE('',*,*,#2027,.F.);
#2603=ORIENTED_EDGE('',*,*,#2028,.T.);
#2604=ORIENTED_EDGE('',*,*,#2029,.F.);
#2605=ORIENTED_EDGE('',*,*,#2028,.F.);
#2606=ORIENTED_EDGE('',*,*,#2030,.F.);
#2607=ORIENTED_EDGE('',*,*,#2031,.T.);
#2608=ORIENTED_EDGE('',*,*,#2032,.F.);
#2609=ORIENTED_EDGE('',*,*,#2031,.F.);
#2610=ORIENTED_EDGE('',*,*,#2033,.F.);
#2611=ORIENTED_EDGE('',*,*,#2034,.T.);
#2612=ORIENTED_EDGE('',*,*,#2035,.F.);
#2613=ORIENTED_EDGE('',*,*,#2034,.F.);
#2614=ORIENTED_EDGE('',*,*,#2036,.F.);
#2615=ORIENTED_EDGE('',*,*,#2037,.T.);
#2616=ORIENTED_EDGE('',*,*,#2038,.F.);
#2617=ORIENTED_EDGE('',*,*,#2037,.F.);
#2618=ORIENTED_EDGE('',*,*,#2039,.F.);
#2619=ORIENTED_EDGE('',*,*,#2040,.T.);
#2620=ORIENTED_EDGE('',*,*,#2041,.F.);
#2621=ORIENTED_EDGE('',*,*,#2040,.F.);
#2622=ORIENTED_EDGE('',*,*,#2042,.F.);
#2623=ORIENTED_EDGE('',*,*,#2043,.T.);
#2624=ORIENTED_EDGE('',*,*,#2044,.F.);
#2625=ORIENTED_EDGE('',*,*,#2043,.F.);
#2626=ORIENTED_EDGE('',*,*,#2045,.F.);
#2627=ORIENTED_EDGE('',*,*,#2046,.T.);
#2628=ORIENTED_EDGE('',*,*,#2047,.F.);
#2629=ORIENTED_EDGE('',*,*,#2046,.F.);
#2630=ORIENTED_EDGE('',*,*,#2048,.F.);
#2631=ORIENTED_EDGE('',*,*,#2049,.T.);
#2632=ORIENTED_EDGE('',*,*,#2050,.F.);
#2633=ORIENTED_EDGE('',*,*,#2049,.F.);
#2634=ORIENTED_EDGE('',*,*,#2051,.F.);
#2635=ORIENTED_EDGE('',*,*,#2052,.T.);
#2636=ORIENTED_EDGE('',*,*,#2053,.F.);
#2637=ORIENTED_EDGE('',*,*,#2052,.F.);
#2638=ORIENTED_EDGE('',*,*,#2054,.F.);
#2639=ORIENTED_EDGE('',*,*,#2055,.T.);
#2640=ORIENTED_EDGE('',*,*,#2056,.F.);
#2641=ORIENTED_EDGE('',*,*,#2055,.F.);
#2642=ORIENTED_EDGE('',*,*,#2057,.F.);
#2643=ORIENTED_EDGE('',*,*,#2058,.T.);
#2644=ORIENTED_EDGE('',*,*,#2059,.F.);
#2645=ORIENTED_EDGE('',*,*,#2058,.F.);
#2646=ORIENTED_EDGE('',*,*,#2007,.T.);
#2647=ORIENTED_EDGE('',*,*,#2059,.T.);
#2648=ORIENTED_EDGE('',*,*,#2056,.T.);
#2649=ORIENTED_EDGE('',*,*,#2053,.T.);
#2650=ORIENTED_EDGE('',*,*,#2050,.T.);
#2651=ORIENTED_EDGE('',*,*,#2047,.T.);
#2652=ORIENTED_EDGE('',*,*,#2044,.T.);
#2653=ORIENTED_EDGE('',*,*,#2041,.T.);
#2654=ORIENTED_EDGE('',*,*,#2038,.T.);
#2655=ORIENTED_EDGE('',*,*,#2035,.T.);
#2656=ORIENTED_EDGE('',*,*,#2032,.T.);
#2657=ORIENTED_EDGE('',*,*,#2029,.T.);
#2658=ORIENTED_EDGE('',*,*,#2026,.T.);
#2659=ORIENTED_EDGE('',*,*,#2023,.T.);
#2660=ORIENTED_EDGE('',*,*,#2020,.T.);
#2661=ORIENTED_EDGE('',*,*,#2017,.T.);
#2662=ORIENTED_EDGE('',*,*,#2014,.T.);
#2663=ORIENTED_EDGE('',*,*,#2011,.T.);
#2664=ORIENTED_EDGE('',*,*,#2003,.T.);
#2665=ORIENTED_EDGE('',*,*,#2004,.T.);
#2666=ORIENTED_EDGE('',*,*,#1997,.T.);
#2667=ORIENTED_EDGE('',*,*,#2008,.F.);
#2668=ORIENTED_EDGE('',*,*,#1999,.F.);
#2669=ORIENTED_EDGE('',*,*,#2015,.T.);
#2670=ORIENTED_EDGE('',*,*,#2030,.T.);
#2671=ORIENTED_EDGE('',*,*,#2042,.T.);
#2672=ORIENTED_EDGE('',*,*,#2057,.T.);
#2673=ORIENTED_EDGE('',*,*,#2033,.T.);
#2674=ORIENTED_EDGE('',*,*,#2027,.T.);
#2675=ORIENTED_EDGE('',*,*,#2024,.T.);
#2676=ORIENTED_EDGE('',*,*,#2021,.T.);
#2677=ORIENTED_EDGE('',*,*,#2018,.T.);
#2678=ORIENTED_EDGE('',*,*,#2009,.T.);
#2679=ORIENTED_EDGE('',*,*,#2012,.T.);
#2680=ORIENTED_EDGE('',*,*,#2036,.T.);
#2681=ORIENTED_EDGE('',*,*,#2039,.T.);
#2682=ORIENTED_EDGE('',*,*,#2045,.T.);
#2683=ORIENTED_EDGE('',*,*,#2048,.T.);
#2684=ORIENTED_EDGE('',*,*,#2051,.T.);
#2685=ORIENTED_EDGE('',*,*,#2054,.T.);
#2686=ORIENTED_EDGE('',*,*,#2060,.F.);
#2687=ORIENTED_EDGE('',*,*,#2061,.F.);
#2688=ORIENTED_EDGE('',*,*,#2062,.F.);
#2689=ORIENTED_EDGE('',*,*,#2063,.F.);
#2690=ORIENTED_EDGE('',*,*,#2064,.T.);
#2691=ORIENTED_EDGE('',*,*,#2065,.T.);
#2692=ORIENTED_EDGE('',*,*,#2066,.T.);
#2693=ORIENTED_EDGE('',*,*,#2067,.T.);
#2694=ORIENTED_EDGE('',*,*,#2061,.T.);
#2695=ORIENTED_EDGE('',*,*,#2068,.T.);
#2696=ORIENTED_EDGE('',*,*,#2069,.F.);
#2697=ORIENTED_EDGE('',*,*,#2070,.F.);
#2698=ORIENTED_EDGE('',*,*,#2071,.F.);
#2699=ORIENTED_EDGE('',*,*,#2065,.F.);
#2700=ORIENTED_EDGE('',*,*,#2070,.T.);
#2701=ORIENTED_EDGE('',*,*,#2072,.F.);
#2702=ORIENTED_EDGE('',*,*,#2063,.T.);
#2703=ORIENTED_EDGE('',*,*,#2073,.F.);
#2704=ORIENTED_EDGE('',*,*,#2074,.T.);
#2705=ORIENTED_EDGE('',*,*,#2075,.T.);
#2706=ORIENTED_EDGE('',*,*,#2076,.T.);
#2707=ORIENTED_EDGE('',*,*,#2077,.T.);
#2708=ORIENTED_EDGE('',*,*,#2075,.F.);
#2709=ORIENTED_EDGE('',*,*,#2076,.F.);
#2710=ORIENTED_EDGE('',*,*,#2077,.F.);
#2711=ORIENTED_EDGE('',*,*,#2078,.T.);
#2712=ORIENTED_EDGE('',*,*,#2079,.T.);
#2713=ORIENTED_EDGE('',*,*,#2078,.F.);
#2714=ORIENTED_EDGE('',*,*,#2074,.F.);
#2715=ORIENTED_EDGE('',*,*,#2079,.F.);
#2716=ORIENTED_EDGE('',*,*,#2080,.T.);
#2717=ORIENTED_EDGE('',*,*,#2068,.F.);
#2718=ORIENTED_EDGE('',*,*,#2060,.T.);
#2719=ORIENTED_EDGE('',*,*,#2073,.T.);
#2720=ORIENTED_EDGE('',*,*,#2062,.T.);
#2721=ORIENTED_EDGE('',*,*,#2067,.F.);
#2722=ORIENTED_EDGE('',*,*,#2066,.F.);
#2723=ORIENTED_EDGE('',*,*,#2071,.T.);
#2724=ORIENTED_EDGE('',*,*,#2072,.T.);
#2725=ORIENTED_EDGE('',*,*,#2069,.T.);
#2726=ORIENTED_EDGE('',*,*,#2064,.F.);
#2727=ORIENTED_EDGE('',*,*,#2080,.F.);
#2728=ORIENTED_EDGE('',*,*,#2081,.F.);
#2729=ORIENTED_EDGE('',*,*,#2082,.T.);
#2730=ORIENTED_EDGE('',*,*,#2083,.T.);
#2731=ORIENTED_EDGE('',*,*,#2082,.F.);
#2732=ORIENTED_EDGE('',*,*,#2083,.F.);
#2733=ORIENTED_EDGE('',*,*,#2084,.F.);
#2734=ORIENTED_EDGE('',*,*,#2085,.F.);
#2735=ORIENTED_EDGE('',*,*,#2086,.F.);
#2736=ORIENTED_EDGE('',*,*,#2087,.F.);
#2737=ORIENTED_EDGE('',*,*,#2088,.F.);
#2738=ORIENTED_EDGE('',*,*,#2089,.F.);
#2739=ORIENTED_EDGE('',*,*,#2090,.F.);
#2740=ORIENTED_EDGE('',*,*,#2091,.F.);
#2741=ORIENTED_EDGE('',*,*,#2092,.F.);
#2742=ORIENTED_EDGE('',*,*,#2093,.F.);
#2743=ORIENTED_EDGE('',*,*,#2094,.F.);
#2744=ORIENTED_EDGE('',*,*,#2095,.F.);
#2745=ORIENTED_EDGE('',*,*,#2096,.F.);
#2746=ORIENTED_EDGE('',*,*,#2097,.F.);
#2747=ORIENTED_EDGE('',*,*,#2098,.F.);
#2748=ORIENTED_EDGE('',*,*,#2099,.F.);
#2749=ORIENTED_EDGE('',*,*,#2100,.F.);
#2750=ORIENTED_EDGE('',*,*,#2101,.F.);
#2751=ORIENTED_EDGE('',*,*,#2102,.F.);
#2752=ORIENTED_EDGE('',*,*,#2103,.F.);
#2753=ORIENTED_EDGE('',*,*,#2104,.F.);
#2754=ORIENTED_EDGE('',*,*,#2105,.F.);
#2755=ORIENTED_EDGE('',*,*,#2106,.F.);
#2756=ORIENTED_EDGE('',*,*,#2107,.F.);
#2757=ORIENTED_EDGE('',*,*,#2108,.F.);
#2758=ORIENTED_EDGE('',*,*,#2109,.F.);
#2759=ORIENTED_EDGE('',*,*,#2110,.F.);
#2760=ORIENTED_EDGE('',*,*,#2111,.F.);
#2761=ORIENTED_EDGE('',*,*,#2112,.F.);
#2762=ORIENTED_EDGE('',*,*,#2113,.F.);
#2763=ORIENTED_EDGE('',*,*,#2114,.F.);
#2764=ORIENTED_EDGE('',*,*,#2115,.F.);
#2765=ORIENTED_EDGE('',*,*,#2116,.F.);
#2766=ORIENTED_EDGE('',*,*,#2117,.F.);
#2767=ORIENTED_EDGE('',*,*,#2118,.F.);
#2768=ORIENTED_EDGE('',*,*,#2119,.F.);
#2769=ORIENTED_EDGE('',*,*,#2120,.F.);
#2770=ORIENTED_EDGE('',*,*,#2121,.F.);
#2771=ORIENTED_EDGE('',*,*,#2122,.F.);
#2772=ORIENTED_EDGE('',*,*,#2123,.F.);
#2773=ORIENTED_EDGE('',*,*,#2124,.F.);
#2774=ORIENTED_EDGE('',*,*,#2125,.F.);
#2775=ORIENTED_EDGE('',*,*,#2126,.F.);
#2776=ORIENTED_EDGE('',*,*,#2127,.F.);
#2777=ORIENTED_EDGE('',*,*,#2128,.F.);
#2778=ORIENTED_EDGE('',*,*,#2129,.F.);
#2779=ORIENTED_EDGE('',*,*,#2130,.F.);
#2780=ORIENTED_EDGE('',*,*,#2131,.F.);
#2781=ORIENTED_EDGE('',*,*,#2132,.F.);
#2782=ORIENTED_EDGE('',*,*,#2133,.F.);
#2783=ORIENTED_EDGE('',*,*,#2134,.F.);
#2784=ORIENTED_EDGE('',*,*,#2135,.F.);
#2785=ORIENTED_EDGE('',*,*,#2136,.F.);
#2786=ORIENTED_EDGE('',*,*,#2137,.F.);
#2787=ORIENTED_EDGE('',*,*,#2138,.F.);
#2788=ORIENTED_EDGE('',*,*,#2139,.F.);
#2789=ORIENTED_EDGE('',*,*,#2140,.F.);
#2790=ORIENTED_EDGE('',*,*,#2141,.F.);
#2791=ORIENTED_EDGE('',*,*,#2142,.F.);
#2792=ORIENTED_EDGE('',*,*,#2143,.F.);
#2793=ORIENTED_EDGE('',*,*,#2144,.F.);
#2794=ORIENTED_EDGE('',*,*,#2145,.F.);
#2795=ORIENTED_EDGE('',*,*,#2146,.F.);
#2796=ORIENTED_EDGE('',*,*,#2147,.F.);
#2797=ORIENTED_EDGE('',*,*,#2148,.F.);
#2798=ORIENTED_EDGE('',*,*,#2149,.F.);
#2799=ORIENTED_EDGE('',*,*,#2150,.F.);
#2800=ORIENTED_EDGE('',*,*,#2151,.F.);
#2801=ORIENTED_EDGE('',*,*,#2152,.F.);
#2802=ORIENTED_EDGE('',*,*,#2153,.F.);
#2803=ORIENTED_EDGE('',*,*,#2154,.F.);
#2804=ORIENTED_EDGE('',*,*,#2155,.F.);
#2805=ORIENTED_EDGE('',*,*,#2156,.F.);
#2806=ORIENTED_EDGE('',*,*,#2157,.F.);
#2807=ORIENTED_EDGE('',*,*,#2158,.F.);
#2808=ORIENTED_EDGE('',*,*,#2159,.F.);
#2809=ORIENTED_EDGE('',*,*,#2160,.F.);
#2810=ORIENTED_EDGE('',*,*,#2161,.T.);
#2811=ORIENTED_EDGE('',*,*,#2162,.F.);
#2812=ORIENTED_EDGE('',*,*,#2163,.F.);
#2813=ORIENTED_EDGE('',*,*,#2157,.T.);
#2814=ORIENTED_EDGE('',*,*,#2164,.F.);
#2815=ORIENTED_EDGE('',*,*,#2165,.F.);
#2816=ORIENTED_EDGE('',*,*,#2166,.T.);
#2817=ORIENTED_EDGE('',*,*,#2167,.F.);
#2818=ORIENTED_EDGE('',*,*,#2153,.T.);
#2819=ORIENTED_EDGE('',*,*,#2168,.F.);
#2820=ORIENTED_EDGE('',*,*,#2169,.T.);
#2821=ORIENTED_EDGE('',*,*,#2170,.F.);
#2822=ORIENTED_EDGE('',*,*,#2149,.T.);
#2823=ORIENTED_EDGE('',*,*,#2171,.F.);
#2824=ORIENTED_EDGE('',*,*,#2172,.T.);
#2825=ORIENTED_EDGE('',*,*,#2173,.F.);
#2826=ORIENTED_EDGE('',*,*,#2145,.T.);
#2827=ORIENTED_EDGE('',*,*,#2174,.F.);
#2828=ORIENTED_EDGE('',*,*,#2175,.T.);
#2829=ORIENTED_EDGE('',*,*,#2176,.F.);
#2830=ORIENTED_EDGE('',*,*,#2141,.T.);
#2831=ORIENTED_EDGE('',*,*,#2177,.F.);
#2832=ORIENTED_EDGE('',*,*,#2178,.T.);
#2833=ORIENTED_EDGE('',*,*,#2179,.F.);
#2834=ORIENTED_EDGE('',*,*,#2137,.T.);
#2835=ORIENTED_EDGE('',*,*,#2180,.F.);
#2836=ORIENTED_EDGE('',*,*,#2181,.T.);
#2837=ORIENTED_EDGE('',*,*,#2182,.F.);
#2838=ORIENTED_EDGE('',*,*,#2133,.T.);
#2839=ORIENTED_EDGE('',*,*,#2183,.F.);
#2840=ORIENTED_EDGE('',*,*,#2184,.T.);
#2841=ORIENTED_EDGE('',*,*,#2185,.F.);
#2842=ORIENTED_EDGE('',*,*,#2129,.T.);
#2843=ORIENTED_EDGE('',*,*,#2186,.F.);
#2844=ORIENTED_EDGE('',*,*,#2187,.T.);
#2845=ORIENTED_EDGE('',*,*,#2188,.F.);
#2846=ORIENTED_EDGE('',*,*,#2125,.T.);
#2847=ORIENTED_EDGE('',*,*,#2189,.F.);
#2848=ORIENTED_EDGE('',*,*,#2190,.T.);
#2849=ORIENTED_EDGE('',*,*,#2191,.F.);
#2850=ORIENTED_EDGE('',*,*,#2121,.T.);
#2851=ORIENTED_EDGE('',*,*,#2192,.F.);
#2852=ORIENTED_EDGE('',*,*,#2193,.T.);
#2853=ORIENTED_EDGE('',*,*,#2194,.F.);
#2854=ORIENTED_EDGE('',*,*,#2117,.T.);
#2855=ORIENTED_EDGE('',*,*,#2195,.F.);
#2856=ORIENTED_EDGE('',*,*,#2196,.T.);
#2857=ORIENTED_EDGE('',*,*,#2197,.F.);
#2858=ORIENTED_EDGE('',*,*,#2113,.T.);
#2859=ORIENTED_EDGE('',*,*,#2198,.F.);
#2860=ORIENTED_EDGE('',*,*,#2199,.T.);
#2861=ORIENTED_EDGE('',*,*,#2200,.F.);
#2862=ORIENTED_EDGE('',*,*,#2109,.T.);
#2863=ORIENTED_EDGE('',*,*,#2201,.F.);
#2864=ORIENTED_EDGE('',*,*,#2202,.T.);
#2865=ORIENTED_EDGE('',*,*,#2203,.F.);
#2866=ORIENTED_EDGE('',*,*,#2105,.T.);
#2867=ORIENTED_EDGE('',*,*,#2204,.F.);
#2868=ORIENTED_EDGE('',*,*,#2205,.T.);
#2869=ORIENTED_EDGE('',*,*,#2206,.F.);
#2870=ORIENTED_EDGE('',*,*,#2101,.T.);
#2871=ORIENTED_EDGE('',*,*,#2207,.F.);
#2872=ORIENTED_EDGE('',*,*,#2208,.T.);
#2873=ORIENTED_EDGE('',*,*,#2209,.F.);
#2874=ORIENTED_EDGE('',*,*,#2097,.T.);
#2875=ORIENTED_EDGE('',*,*,#2210,.F.);
#2876=ORIENTED_EDGE('',*,*,#2211,.T.);
#2877=ORIENTED_EDGE('',*,*,#2212,.F.);
#2878=ORIENTED_EDGE('',*,*,#2093,.T.);
#2879=ORIENTED_EDGE('',*,*,#2213,.F.);
#2880=ORIENTED_EDGE('',*,*,#2214,.T.);
#2881=ORIENTED_EDGE('',*,*,#2215,.F.);
#2882=ORIENTED_EDGE('',*,*,#2089,.T.);
#2883=ORIENTED_EDGE('',*,*,#2216,.F.);
#2884=ORIENTED_EDGE('',*,*,#2217,.T.);
#2885=ORIENTED_EDGE('',*,*,#2218,.F.);
#2886=ORIENTED_EDGE('',*,*,#2085,.T.);
#2887=ORIENTED_EDGE('',*,*,#2219,.F.);
#2888=ORIENTED_EDGE('',*,*,#2220,.F.);
#2889=ORIENTED_EDGE('',*,*,#2221,.F.);
#2890=ORIENTED_EDGE('',*,*,#2178,.F.);
#2891=ORIENTED_EDGE('',*,*,#2222,.F.);
#2892=ORIENTED_EDGE('',*,*,#2223,.F.);
#2893=ORIENTED_EDGE('',*,*,#2224,.F.);
#2894=ORIENTED_EDGE('',*,*,#2202,.F.);
#2895=ORIENTED_EDGE('',*,*,#2225,.F.);
#2896=ORIENTED_EDGE('',*,*,#2226,.F.);
#2897=ORIENTED_EDGE('',*,*,#2227,.F.);
#2898=ORIENTED_EDGE('',*,*,#2205,.F.);
#2899=ORIENTED_EDGE('',*,*,#2228,.F.);
#2900=ORIENTED_EDGE('',*,*,#2229,.F.);
#2901=ORIENTED_EDGE('',*,*,#2230,.F.);
#2902=ORIENTED_EDGE('',*,*,#2175,.F.);
#2903=ORIENTED_EDGE('',*,*,#2231,.F.);
#2904=ORIENTED_EDGE('',*,*,#2232,.F.);
#2905=ORIENTED_EDGE('',*,*,#2233,.F.);
#2906=ORIENTED_EDGE('',*,*,#2217,.F.);
#2907=ORIENTED_EDGE('',*,*,#2234,.F.);
#2908=ORIENTED_EDGE('',*,*,#2235,.F.);
#2909=ORIENTED_EDGE('',*,*,#2236,.F.);
#2910=ORIENTED_EDGE('',*,*,#2199,.F.);
#2911=ORIENTED_EDGE('',*,*,#2237,.F.);
#2912=ORIENTED_EDGE('',*,*,#2238,.F.);
#2913=ORIENTED_EDGE('',*,*,#2239,.F.);
#2914=ORIENTED_EDGE('',*,*,#2172,.F.);
#2915=ORIENTED_EDGE('',*,*,#2240,.F.);
#2916=ORIENTED_EDGE('',*,*,#2241,.F.);
#2917=ORIENTED_EDGE('',*,*,#2242,.F.);
#2918=ORIENTED_EDGE('',*,*,#2169,.F.);
#2919=ORIENTED_EDGE('',*,*,#2243,.F.);
#2920=ORIENTED_EDGE('',*,*,#2244,.F.);
#2921=ORIENTED_EDGE('',*,*,#2245,.F.);
#2922=ORIENTED_EDGE('',*,*,#2196,.F.);
#2923=ORIENTED_EDGE('',*,*,#2246,.F.);
#2924=ORIENTED_EDGE('',*,*,#2247,.F.);
#2925=ORIENTED_EDGE('',*,*,#2248,.F.);
#2926=ORIENTED_EDGE('',*,*,#2193,.F.);
#2927=ORIENTED_EDGE('',*,*,#2249,.F.);
#2928=ORIENTED_EDGE('',*,*,#2250,.F.);
#2929=ORIENTED_EDGE('',*,*,#2251,.F.);
#2930=ORIENTED_EDGE('',*,*,#2166,.F.);
#2931=ORIENTED_EDGE('',*,*,#2252,.F.);
#2932=ORIENTED_EDGE('',*,*,#2253,.F.);
#2933=ORIENTED_EDGE('',*,*,#2254,.F.);
#2934=ORIENTED_EDGE('',*,*,#2161,.F.);
#2935=ORIENTED_EDGE('',*,*,#2255,.F.);
#2936=ORIENTED_EDGE('',*,*,#2256,.F.);
#2937=ORIENTED_EDGE('',*,*,#2257,.F.);
#2938=ORIENTED_EDGE('',*,*,#2190,.F.);
#2939=ORIENTED_EDGE('',*,*,#2258,.F.);
#2940=ORIENTED_EDGE('',*,*,#2259,.F.);
#2941=ORIENTED_EDGE('',*,*,#2260,.F.);
#2942=ORIENTED_EDGE('',*,*,#2187,.F.);
#2943=ORIENTED_EDGE('',*,*,#2261,.F.);
#2944=ORIENTED_EDGE('',*,*,#2262,.F.);
#2945=ORIENTED_EDGE('',*,*,#2263,.F.);
#2946=ORIENTED_EDGE('',*,*,#2214,.F.);
#2947=ORIENTED_EDGE('',*,*,#2264,.F.);
#2948=ORIENTED_EDGE('',*,*,#2265,.F.);
#2949=ORIENTED_EDGE('',*,*,#2266,.F.);
#2950=ORIENTED_EDGE('',*,*,#2211,.F.);
#2951=ORIENTED_EDGE('',*,*,#2267,.F.);
#2952=ORIENTED_EDGE('',*,*,#2268,.F.);
#2953=ORIENTED_EDGE('',*,*,#2269,.F.);
#2954=ORIENTED_EDGE('',*,*,#2184,.F.);
#2955=ORIENTED_EDGE('',*,*,#2270,.F.);
#2956=ORIENTED_EDGE('',*,*,#2271,.F.);
#2957=ORIENTED_EDGE('',*,*,#2272,.F.);
#2958=ORIENTED_EDGE('',*,*,#2208,.F.);
#2959=ORIENTED_EDGE('',*,*,#2273,.F.);
#2960=ORIENTED_EDGE('',*,*,#2274,.F.);
#2961=ORIENTED_EDGE('',*,*,#2275,.F.);
#2962=ORIENTED_EDGE('',*,*,#2181,.F.);
#2963=ORIENTED_EDGE('',*,*,#2276,.F.);
#2964=ORIENTED_EDGE('',*,*,#2277,.T.);
#2965=ORIENTED_EDGE('',*,*,#2164,.T.);
#2966=ORIENTED_EDGE('',*,*,#2156,.T.);
#2967=ORIENTED_EDGE('',*,*,#2278,.T.);
#2968=ORIENTED_EDGE('',*,*,#2249,.T.);
#2969=ORIENTED_EDGE('',*,*,#2165,.T.);
#2970=ORIENTED_EDGE('',*,*,#2152,.T.);
#2971=ORIENTED_EDGE('',*,*,#2279,.T.);
#2972=ORIENTED_EDGE('',*,*,#2240,.T.);
#2973=ORIENTED_EDGE('',*,*,#2168,.T.);
#2974=ORIENTED_EDGE('',*,*,#2148,.T.);
#2975=ORIENTED_EDGE('',*,*,#2280,.T.);
#2976=ORIENTED_EDGE('',*,*,#2237,.T.);
#2977=ORIENTED_EDGE('',*,*,#2171,.T.);
#2978=ORIENTED_EDGE('',*,*,#2144,.T.);
#2979=ORIENTED_EDGE('',*,*,#2281,.T.);
#2980=ORIENTED_EDGE('',*,*,#2228,.T.);
#2981=ORIENTED_EDGE('',*,*,#2174,.T.);
#2982=ORIENTED_EDGE('',*,*,#2140,.T.);
#2983=ORIENTED_EDGE('',*,*,#2282,.T.);
#2984=ORIENTED_EDGE('',*,*,#2283,.T.);
#2985=ORIENTED_EDGE('',*,*,#2284,.T.);
#2986=ORIENTED_EDGE('',*,*,#2285,.T.);
#2987=ORIENTED_EDGE('',*,*,#2286,.T.);
#2988=ORIENTED_EDGE('',*,*,#2219,.T.);
#2989=ORIENTED_EDGE('',*,*,#2177,.T.);
#2990=ORIENTED_EDGE('',*,*,#2136,.T.);
#2991=ORIENTED_EDGE('',*,*,#2287,.T.);
#2992=ORIENTED_EDGE('',*,*,#2273,.T.);
#2993=ORIENTED_EDGE('',*,*,#2180,.T.);
#2994=ORIENTED_EDGE('',*,*,#2132,.T.);
#2995=ORIENTED_EDGE('',*,*,#2288,.T.);
#2996=ORIENTED_EDGE('',*,*,#2267,.T.);
#2997=ORIENTED_EDGE('',*,*,#2183,.T.);
#2998=ORIENTED_EDGE('',*,*,#2128,.T.);
#2999=ORIENTED_EDGE('',*,*,#2289,.T.);
#3000=ORIENTED_EDGE('',*,*,#2258,.T.);
#3001=ORIENTED_EDGE('',*,*,#2186,.T.);
#3002=ORIENTED_EDGE('',*,*,#2124,.T.);
#3003=ORIENTED_EDGE('',*,*,#2290,.T.);
#3004=ORIENTED_EDGE('',*,*,#2255,.T.);
#3005=ORIENTED_EDGE('',*,*,#2189,.T.);
#3006=ORIENTED_EDGE('',*,*,#2120,.T.);
#3007=ORIENTED_EDGE('',*,*,#2291,.T.);
#3008=ORIENTED_EDGE('',*,*,#2246,.T.);
#3009=ORIENTED_EDGE('',*,*,#2192,.T.);
#3010=ORIENTED_EDGE('',*,*,#2116,.T.);
#3011=ORIENTED_EDGE('',*,*,#2292,.T.);
#3012=ORIENTED_EDGE('',*,*,#2243,.T.);
#3013=ORIENTED_EDGE('',*,*,#2195,.T.);
#3014=ORIENTED_EDGE('',*,*,#2112,.T.);
#3015=ORIENTED_EDGE('',*,*,#2293,.T.);
#3016=ORIENTED_EDGE('',*,*,#2234,.T.);
#3017=ORIENTED_EDGE('',*,*,#2198,.T.);
#3018=ORIENTED_EDGE('',*,*,#2108,.T.);
#3019=ORIENTED_EDGE('',*,*,#2294,.T.);
#3020=ORIENTED_EDGE('',*,*,#2231,.T.);
#3021=ORIENTED_EDGE('',*,*,#2216,.T.);
#3022=ORIENTED_EDGE('',*,*,#2084,.T.);
#3023=ORIENTED_EDGE('',*,*,#2295,.T.);
#3024=ORIENTED_EDGE('',*,*,#2222,.T.);
#3025=ORIENTED_EDGE('',*,*,#2201,.T.);
#3026=ORIENTED_EDGE('',*,*,#2104,.T.);
#3027=ORIENTED_EDGE('',*,*,#2296,.T.);
#3028=ORIENTED_EDGE('',*,*,#2225,.T.);
#3029=ORIENTED_EDGE('',*,*,#2204,.T.);
#3030=ORIENTED_EDGE('',*,*,#2100,.T.);
#3031=ORIENTED_EDGE('',*,*,#2297,.T.);
#3032=ORIENTED_EDGE('',*,*,#2270,.T.);
#3033=ORIENTED_EDGE('',*,*,#2207,.T.);
#3034=ORIENTED_EDGE('',*,*,#2096,.T.);
#3035=ORIENTED_EDGE('',*,*,#2298,.T.);
#3036=ORIENTED_EDGE('',*,*,#2264,.T.);
#3037=ORIENTED_EDGE('',*,*,#2210,.T.);
#3038=ORIENTED_EDGE('',*,*,#2092,.T.);
#3039=ORIENTED_EDGE('',*,*,#2299,.T.);
#3040=ORIENTED_EDGE('',*,*,#2261,.T.);
#3041=ORIENTED_EDGE('',*,*,#2213,.T.);
#3042=ORIENTED_EDGE('',*,*,#2088,.T.);
#3043=ORIENTED_EDGE('',*,*,#2300,.T.);
#3044=ORIENTED_EDGE('',*,*,#2252,.T.);
#3045=ORIENTED_EDGE('',*,*,#2160,.T.);
#3046=ORIENTED_EDGE('',*,*,#2277,.F.);
#3047=ORIENTED_EDGE('',*,*,#2143,.T.);
#3048=ORIENTED_EDGE('',*,*,#2301,.F.);
#3049=ORIENTED_EDGE('',*,*,#2302,.T.);
#3050=ORIENTED_EDGE('',*,*,#2282,.F.);
#3051=ORIENTED_EDGE('',*,*,#2091,.T.);
#3052=ORIENTED_EDGE('',*,*,#2303,.F.);
#3053=ORIENTED_EDGE('',*,*,#2253,.T.);
#3054=ORIENTED_EDGE('',*,*,#2300,.F.);
#3055=ORIENTED_EDGE('',*,*,#2250,.T.);
#3056=ORIENTED_EDGE('',*,*,#2278,.F.);
#3057=ORIENTED_EDGE('',*,*,#2159,.T.);
#3058=ORIENTED_EDGE('',*,*,#2304,.F.);
#3059=ORIENTED_EDGE('',*,*,#2241,.T.);
#3060=ORIENTED_EDGE('',*,*,#2279,.F.);
#3061=ORIENTED_EDGE('',*,*,#2155,.T.);
#3062=ORIENTED_EDGE('',*,*,#2305,.F.);
#3063=ORIENTED_EDGE('',*,*,#2238,.T.);
#3064=ORIENTED_EDGE('',*,*,#2280,.F.);
#3065=ORIENTED_EDGE('',*,*,#2151,.T.);
#3066=ORIENTED_EDGE('',*,*,#2306,.F.);
#3067=ORIENTED_EDGE('',*,*,#2229,.T.);
#3068=ORIENTED_EDGE('',*,*,#2281,.F.);
#3069=ORIENTED_EDGE('',*,*,#2147,.T.);
#3070=ORIENTED_EDGE('',*,*,#2307,.F.);
#3071=ORIENTED_EDGE('',*,*,#2220,.T.);
#3072=ORIENTED_EDGE('',*,*,#2286,.F.);
#3073=ORIENTED_EDGE('',*,*,#2308,.T.);
#3074=ORIENTED_EDGE('',*,*,#2309,.F.);
#3075=ORIENTED_EDGE('',*,*,#2274,.T.);
#3076=ORIENTED_EDGE('',*,*,#2287,.F.);
#3077=ORIENTED_EDGE('',*,*,#2139,.T.);
#3078=ORIENTED_EDGE('',*,*,#2310,.F.);
#3079=ORIENTED_EDGE('',*,*,#2268,.T.);
#3080=ORIENTED_EDGE('',*,*,#2288,.F.);
#3081=ORIENTED_EDGE('',*,*,#2135,.T.);
#3082=ORIENTED_EDGE('',*,*,#2311,.F.);
#3083=ORIENTED_EDGE('',*,*,#2259,.T.);
#3084=ORIENTED_EDGE('',*,*,#2289,.F.);
#3085=ORIENTED_EDGE('',*,*,#2131,.T.);
#3086=ORIENTED_EDGE('',*,*,#2312,.F.);
#3087=ORIENTED_EDGE('',*,*,#2256,.T.);
#3088=ORIENTED_EDGE('',*,*,#2290,.F.);
#3089=ORIENTED_EDGE('',*,*,#2127,.T.);
#3090=ORIENTED_EDGE('',*,*,#2313,.F.);
#3091=ORIENTED_EDGE('',*,*,#2247,.T.);
#3092=ORIENTED_EDGE('',*,*,#2291,.F.);
#3093=ORIENTED_EDGE('',*,*,#2123,.T.);
#3094=ORIENTED_EDGE('',*,*,#2314,.F.);
#3095=ORIENTED_EDGE('',*,*,#2244,.T.);
#3096=ORIENTED_EDGE('',*,*,#2292,.F.);
#3097=ORIENTED_EDGE('',*,*,#2119,.T.);
#3098=ORIENTED_EDGE('',*,*,#2315,.F.);
#3099=ORIENTED_EDGE('',*,*,#2235,.T.);
#3100=ORIENTED_EDGE('',*,*,#2293,.F.);
#3101=ORIENTED_EDGE('',*,*,#2115,.T.);
#3102=ORIENTED_EDGE('',*,*,#2316,.F.);
#3103=ORIENTED_EDGE('',*,*,#2087,.T.);
#3104=ORIENTED_EDGE('',*,*,#2317,.F.);
#3105=ORIENTED_EDGE('',*,*,#2223,.T.);
#3106=ORIENTED_EDGE('',*,*,#2295,.F.);
#3107=ORIENTED_EDGE('',*,*,#2226,.T.);
#3108=ORIENTED_EDGE('',*,*,#2296,.F.);
#3109=ORIENTED_EDGE('',*,*,#2107,.T.);
#3110=ORIENTED_EDGE('',*,*,#2318,.F.);
#3111=ORIENTED_EDGE('',*,*,#2271,.T.);
#3112=ORIENTED_EDGE('',*,*,#2297,.F.);
#3113=ORIENTED_EDGE('',*,*,#2103,.T.);
#3114=ORIENTED_EDGE('',*,*,#2319,.F.);
#3115=ORIENTED_EDGE('',*,*,#2265,.T.);
#3116=ORIENTED_EDGE('',*,*,#2298,.F.);
#3117=ORIENTED_EDGE('',*,*,#2099,.T.);
#3118=ORIENTED_EDGE('',*,*,#2320,.F.);
#3119=ORIENTED_EDGE('',*,*,#2262,.T.);
#3120=ORIENTED_EDGE('',*,*,#2299,.F.);
#3121=ORIENTED_EDGE('',*,*,#2095,.T.);
#3122=ORIENTED_EDGE('',*,*,#2321,.F.);
#3123=ORIENTED_EDGE('',*,*,#2285,.F.);
#3124=ORIENTED_EDGE('',*,*,#2322,.F.);
#3125=ORIENTED_EDGE('',*,*,#2323,.F.);
#3126=ORIENTED_EDGE('',*,*,#2308,.F.);
#3127=ORIENTED_EDGE('',*,*,#2284,.F.);
#3128=ORIENTED_EDGE('',*,*,#2324,.T.);
#3129=ORIENTED_EDGE('',*,*,#2325,.F.);
#3130=ORIENTED_EDGE('',*,*,#2322,.T.);
#3131=ORIENTED_EDGE('',*,*,#2283,.F.);
#3132=ORIENTED_EDGE('',*,*,#2302,.F.);
#3133=ORIENTED_EDGE('',*,*,#2326,.F.);
#3134=ORIENTED_EDGE('',*,*,#2324,.F.);
#3135=ORIENTED_EDGE('',*,*,#2327,.F.);
#3136=ORIENTED_EDGE('',*,*,#2328,.T.);
#3137=ORIENTED_EDGE('',*,*,#2162,.T.);
#3138=ORIENTED_EDGE('',*,*,#2254,.T.);
#3139=ORIENTED_EDGE('',*,*,#2303,.T.);
#3140=ORIENTED_EDGE('',*,*,#2090,.T.);
#3141=ORIENTED_EDGE('',*,*,#2215,.T.);
#3142=ORIENTED_EDGE('',*,*,#2263,.T.);
#3143=ORIENTED_EDGE('',*,*,#2321,.T.);
#3144=ORIENTED_EDGE('',*,*,#2094,.T.);
#3145=ORIENTED_EDGE('',*,*,#2212,.T.);
#3146=ORIENTED_EDGE('',*,*,#2266,.T.);
#3147=ORIENTED_EDGE('',*,*,#2320,.T.);
#3148=ORIENTED_EDGE('',*,*,#2098,.T.);
#3149=ORIENTED_EDGE('',*,*,#2209,.T.);
#3150=ORIENTED_EDGE('',*,*,#2272,.T.);
#3151=ORIENTED_EDGE('',*,*,#2319,.T.);
#3152=ORIENTED_EDGE('',*,*,#2102,.T.);
#3153=ORIENTED_EDGE('',*,*,#2206,.T.);
#3154=ORIENTED_EDGE('',*,*,#2227,.T.);
#3155=ORIENTED_EDGE('',*,*,#2318,.T.);
#3156=ORIENTED_EDGE('',*,*,#2106,.T.);
#3157=ORIENTED_EDGE('',*,*,#2203,.T.);
#3158=ORIENTED_EDGE('',*,*,#2224,.T.);
#3159=ORIENTED_EDGE('',*,*,#2317,.T.);
#3160=ORIENTED_EDGE('',*,*,#2086,.T.);
#3161=ORIENTED_EDGE('',*,*,#2218,.T.);
#3162=ORIENTED_EDGE('',*,*,#2233,.T.);
#3163=ORIENTED_EDGE('',*,*,#2329,.T.);
#3164=ORIENTED_EDGE('',*,*,#2110,.T.);
#3165=ORIENTED_EDGE('',*,*,#2200,.T.);
#3166=ORIENTED_EDGE('',*,*,#2236,.T.);
#3167=ORIENTED_EDGE('',*,*,#2316,.T.);
#3168=ORIENTED_EDGE('',*,*,#2114,.T.);
#3169=ORIENTED_EDGE('',*,*,#2197,.T.);
#3170=ORIENTED_EDGE('',*,*,#2245,.T.);
#3171=ORIENTED_EDGE('',*,*,#2315,.T.);
#3172=ORIENTED_EDGE('',*,*,#2118,.T.);
#3173=ORIENTED_EDGE('',*,*,#2194,.T.);
#3174=ORIENTED_EDGE('',*,*,#2248,.T.);
#3175=ORIENTED_EDGE('',*,*,#2314,.T.);
#3176=ORIENTED_EDGE('',*,*,#2122,.T.);
#3177=ORIENTED_EDGE('',*,*,#2191,.T.);
#3178=ORIENTED_EDGE('',*,*,#2257,.T.);
#3179=ORIENTED_EDGE('',*,*,#2313,.T.);
#3180=ORIENTED_EDGE('',*,*,#2126,.T.);
#3181=ORIENTED_EDGE('',*,*,#2188,.T.);
#3182=ORIENTED_EDGE('',*,*,#2260,.T.);
#3183=ORIENTED_EDGE('',*,*,#2312,.T.);
#3184=ORIENTED_EDGE('',*,*,#2130,.T.);
#3185=ORIENTED_EDGE('',*,*,#2185,.T.);
#3186=ORIENTED_EDGE('',*,*,#2269,.T.);
#3187=ORIENTED_EDGE('',*,*,#2311,.T.);
#3188=ORIENTED_EDGE('',*,*,#2134,.T.);
#3189=ORIENTED_EDGE('',*,*,#2182,.T.);
#3190=ORIENTED_EDGE('',*,*,#2275,.T.);
#3191=ORIENTED_EDGE('',*,*,#2310,.T.);
#3192=ORIENTED_EDGE('',*,*,#2138,.T.);
#3193=ORIENTED_EDGE('',*,*,#2179,.T.);
#3194=ORIENTED_EDGE('',*,*,#2221,.T.);
#3195=ORIENTED_EDGE('',*,*,#2309,.T.);
#3196=ORIENTED_EDGE('',*,*,#2323,.T.);
#3197=ORIENTED_EDGE('',*,*,#2325,.T.);
#3198=ORIENTED_EDGE('',*,*,#2326,.T.);
#3199=ORIENTED_EDGE('',*,*,#2301,.T.);
#3200=ORIENTED_EDGE('',*,*,#2142,.T.);
#3201=ORIENTED_EDGE('',*,*,#2176,.T.);
#3202=ORIENTED_EDGE('',*,*,#2230,.T.);
#3203=ORIENTED_EDGE('',*,*,#2307,.T.);
#3204=ORIENTED_EDGE('',*,*,#2146,.T.);
#3205=ORIENTED_EDGE('',*,*,#2173,.T.);
#3206=ORIENTED_EDGE('',*,*,#2239,.T.);
#3207=ORIENTED_EDGE('',*,*,#2306,.T.);
#3208=ORIENTED_EDGE('',*,*,#2150,.T.);
#3209=ORIENTED_EDGE('',*,*,#2170,.T.);
#3210=ORIENTED_EDGE('',*,*,#2242,.T.);
#3211=ORIENTED_EDGE('',*,*,#2305,.T.);
#3212=ORIENTED_EDGE('',*,*,#2154,.T.);
#3213=ORIENTED_EDGE('',*,*,#2167,.T.);
#3214=ORIENTED_EDGE('',*,*,#2251,.T.);
#3215=ORIENTED_EDGE('',*,*,#2304,.T.);
#3216=ORIENTED_EDGE('',*,*,#2158,.T.);
#3217=ORIENTED_EDGE('',*,*,#2163,.T.);
#3218=ORIENTED_EDGE('',*,*,#2328,.F.);
#3219=ORIENTED_EDGE('',*,*,#2081,.T.);
#3220=ORIENTED_EDGE('',*,*,#2327,.T.);
#3221=ORIENTED_EDGE('',*,*,#2276,.T.);
#3222=ORIENTED_EDGE('',*,*,#2232,.T.);
#3223=ORIENTED_EDGE('',*,*,#2294,.F.);
#3224=ORIENTED_EDGE('',*,*,#2111,.T.);
#3225=ORIENTED_EDGE('',*,*,#2329,.F.);
#3226=ORIENTED_EDGE('',*,*,#2330,.F.);
#3227=ORIENTED_EDGE('',*,*,#2331,.F.);
#3228=ORIENTED_EDGE('',*,*,#2332,.F.);
#3229=ORIENTED_EDGE('',*,*,#2333,.F.);
#3230=ORIENTED_EDGE('',*,*,#2334,.F.);
#3231=ORIENTED_EDGE('',*,*,#2335,.F.);
#3232=ORIENTED_EDGE('',*,*,#2336,.F.);
#3233=ORIENTED_EDGE('',*,*,#2337,.F.);
#3234=ORIENTED_EDGE('',*,*,#2330,.T.);
#3235=ORIENTED_EDGE('',*,*,#2338,.F.);
#3236=ORIENTED_EDGE('',*,*,#2334,.T.);
#3237=ORIENTED_EDGE('',*,*,#2339,.F.);
#3238=ORIENTED_EDGE('',*,*,#2340,.T.);
#3239=ORIENTED_EDGE('',*,*,#2341,.T.);
#3240=ORIENTED_EDGE('',*,*,#2342,.F.);
#3241=ORIENTED_EDGE('',*,*,#2343,.T.);
#3242=ORIENTED_EDGE('',*,*,#2340,.F.);
#3243=ORIENTED_EDGE('',*,*,#2343,.F.);
#3244=ORIENTED_EDGE('',*,*,#2342,.T.);
#3245=ORIENTED_EDGE('',*,*,#2344,.F.);
#3246=ORIENTED_EDGE('',*,*,#2345,.T.);
#3247=ORIENTED_EDGE('',*,*,#2341,.F.);
#3248=ORIENTED_EDGE('',*,*,#2345,.F.);
#3249=ORIENTED_EDGE('',*,*,#2344,.T.);
#3250=ORIENTED_EDGE('',*,*,#2331,.T.);
#3251=ORIENTED_EDGE('',*,*,#2339,.T.);
#3252=ORIENTED_EDGE('',*,*,#2337,.T.);
#3253=ORIENTED_EDGE('',*,*,#2346,.F.);
#3254=ORIENTED_EDGE('',*,*,#2333,.T.);
#3255=ORIENTED_EDGE('',*,*,#2347,.F.);
#3256=ORIENTED_EDGE('',*,*,#2335,.T.);
#3257=ORIENTED_EDGE('',*,*,#2338,.T.);
#3258=ORIENTED_EDGE('',*,*,#2332,.T.);
#3259=ORIENTED_EDGE('',*,*,#2346,.T.);
#3260=ORIENTED_EDGE('',*,*,#2336,.T.);
#3261=ORIENTED_EDGE('',*,*,#2347,.T.);
#3262=ORIENTED_EDGE('',*,*,#2348,.F.);
#3263=ORIENTED_EDGE('',*,*,#2349,.F.);
#3264=ORIENTED_EDGE('',*,*,#2350,.F.);
#3265=ORIENTED_EDGE('',*,*,#2351,.F.);
#3266=ORIENTED_EDGE('',*,*,#2352,.F.);
#3267=ORIENTED_EDGE('',*,*,#2353,.F.);
#3268=ORIENTED_EDGE('',*,*,#2354,.F.);
#3269=ORIENTED_EDGE('',*,*,#2355,.F.);
#3270=ORIENTED_EDGE('',*,*,#2348,.T.);
#3271=ORIENTED_EDGE('',*,*,#2356,.F.);
#3272=ORIENTED_EDGE('',*,*,#2352,.T.);
#3273=ORIENTED_EDGE('',*,*,#2357,.F.);
#3274=ORIENTED_EDGE('',*,*,#2358,.T.);
#3275=ORIENTED_EDGE('',*,*,#2359,.T.);
#3276=ORIENTED_EDGE('',*,*,#2360,.F.);
#3277=ORIENTED_EDGE('',*,*,#2361,.T.);
#3278=ORIENTED_EDGE('',*,*,#2358,.F.);
#3279=ORIENTED_EDGE('',*,*,#2361,.F.);
#3280=ORIENTED_EDGE('',*,*,#2360,.T.);
#3281=ORIENTED_EDGE('',*,*,#2362,.F.);
#3282=ORIENTED_EDGE('',*,*,#2363,.T.);
#3283=ORIENTED_EDGE('',*,*,#2359,.F.);
#3284=ORIENTED_EDGE('',*,*,#2363,.F.);
#3285=ORIENTED_EDGE('',*,*,#2362,.T.);
#3286=ORIENTED_EDGE('',*,*,#2349,.T.);
#3287=ORIENTED_EDGE('',*,*,#2357,.T.);
#3288=ORIENTED_EDGE('',*,*,#2355,.T.);
#3289=ORIENTED_EDGE('',*,*,#2364,.F.);
#3290=ORIENTED_EDGE('',*,*,#2351,.T.);
#3291=ORIENTED_EDGE('',*,*,#2365,.F.);
#3292=ORIENTED_EDGE('',*,*,#2353,.T.);
#3293=ORIENTED_EDGE('',*,*,#2356,.T.);
#3294=ORIENTED_EDGE('',*,*,#2350,.T.);
#3295=ORIENTED_EDGE('',*,*,#2364,.T.);
#3296=ORIENTED_EDGE('',*,*,#2354,.T.);
#3297=ORIENTED_EDGE('',*,*,#2365,.T.);
#3298=ORIENTED_EDGE('',*,*,#2366,.F.);
#3299=ORIENTED_EDGE('',*,*,#2367,.F.);
#3300=ORIENTED_EDGE('',*,*,#2368,.F.);
#3301=ORIENTED_EDGE('',*,*,#2369,.F.);
#3302=ORIENTED_EDGE('',*,*,#2370,.F.);
#3303=ORIENTED_EDGE('',*,*,#2371,.F.);
#3304=ORIENTED_EDGE('',*,*,#2372,.F.);
#3305=ORIENTED_EDGE('',*,*,#2373,.F.);
#3306=ORIENTED_EDGE('',*,*,#2366,.T.);
#3307=ORIENTED_EDGE('',*,*,#2374,.F.);
#3308=ORIENTED_EDGE('',*,*,#2370,.T.);
#3309=ORIENTED_EDGE('',*,*,#2375,.F.);
#3310=ORIENTED_EDGE('',*,*,#2376,.T.);
#3311=ORIENTED_EDGE('',*,*,#2377,.T.);
#3312=ORIENTED_EDGE('',*,*,#2378,.F.);
#3313=ORIENTED_EDGE('',*,*,#2379,.T.);
#3314=ORIENTED_EDGE('',*,*,#2376,.F.);
#3315=ORIENTED_EDGE('',*,*,#2379,.F.);
#3316=ORIENTED_EDGE('',*,*,#2378,.T.);
#3317=ORIENTED_EDGE('',*,*,#2380,.F.);
#3318=ORIENTED_EDGE('',*,*,#2381,.T.);
#3319=ORIENTED_EDGE('',*,*,#2377,.F.);
#3320=ORIENTED_EDGE('',*,*,#2381,.F.);
#3321=ORIENTED_EDGE('',*,*,#2380,.T.);
#3322=ORIENTED_EDGE('',*,*,#2367,.T.);
#3323=ORIENTED_EDGE('',*,*,#2375,.T.);
#3324=ORIENTED_EDGE('',*,*,#2373,.T.);
#3325=ORIENTED_EDGE('',*,*,#2382,.F.);
#3326=ORIENTED_EDGE('',*,*,#2369,.T.);
#3327=ORIENTED_EDGE('',*,*,#2383,.F.);
#3328=ORIENTED_EDGE('',*,*,#2371,.T.);
#3329=ORIENTED_EDGE('',*,*,#2374,.T.);
#3330=ORIENTED_EDGE('',*,*,#2368,.T.);
#3331=ORIENTED_EDGE('',*,*,#2382,.T.);
#3332=ORIENTED_EDGE('',*,*,#2372,.T.);
#3333=ORIENTED_EDGE('',*,*,#2383,.T.);
#3334=ORIENTED_EDGE('',*,*,#2384,.F.);
#3335=ORIENTED_EDGE('',*,*,#2385,.F.);
#3336=ORIENTED_EDGE('',*,*,#2386,.F.);
#3337=ORIENTED_EDGE('',*,*,#2387,.F.);
#3338=ORIENTED_EDGE('',*,*,#2388,.F.);
#3339=ORIENTED_EDGE('',*,*,#2389,.F.);
#3340=ORIENTED_EDGE('',*,*,#2390,.F.);
#3341=ORIENTED_EDGE('',*,*,#2391,.F.);
#3342=ORIENTED_EDGE('',*,*,#2384,.T.);
#3343=ORIENTED_EDGE('',*,*,#2392,.F.);
#3344=ORIENTED_EDGE('',*,*,#2388,.T.);
#3345=ORIENTED_EDGE('',*,*,#2393,.F.);
#3346=ORIENTED_EDGE('',*,*,#2394,.T.);
#3347=ORIENTED_EDGE('',*,*,#2395,.T.);
#3348=ORIENTED_EDGE('',*,*,#2396,.F.);
#3349=ORIENTED_EDGE('',*,*,#2397,.T.);
#3350=ORIENTED_EDGE('',*,*,#2394,.F.);
#3351=ORIENTED_EDGE('',*,*,#2397,.F.);
#3352=ORIENTED_EDGE('',*,*,#2396,.T.);
#3353=ORIENTED_EDGE('',*,*,#2398,.F.);
#3354=ORIENTED_EDGE('',*,*,#2399,.T.);
#3355=ORIENTED_EDGE('',*,*,#2395,.F.);
#3356=ORIENTED_EDGE('',*,*,#2399,.F.);
#3357=ORIENTED_EDGE('',*,*,#2398,.T.);
#3358=ORIENTED_EDGE('',*,*,#2385,.T.);
#3359=ORIENTED_EDGE('',*,*,#2393,.T.);
#3360=ORIENTED_EDGE('',*,*,#2391,.T.);
#3361=ORIENTED_EDGE('',*,*,#2400,.F.);
#3362=ORIENTED_EDGE('',*,*,#2387,.T.);
#3363=ORIENTED_EDGE('',*,*,#2401,.F.);
#3364=ORIENTED_EDGE('',*,*,#2389,.T.);
#3365=ORIENTED_EDGE('',*,*,#2392,.T.);
#3366=ORIENTED_EDGE('',*,*,#2386,.T.);
#3367=ORIENTED_EDGE('',*,*,#2400,.T.);
#3368=ORIENTED_EDGE('',*,*,#2390,.T.);
#3369=ORIENTED_EDGE('',*,*,#2401,.T.);
#3370=ORIENTED_EDGE('',*,*,#2402,.F.);
#3371=ORIENTED_EDGE('',*,*,#2403,.F.);
#3372=ORIENTED_EDGE('',*,*,#2404,.F.);
#3373=ORIENTED_EDGE('',*,*,#2405,.F.);
#3374=ORIENTED_EDGE('',*,*,#2406,.F.);
#3375=ORIENTED_EDGE('',*,*,#2407,.F.);
#3376=ORIENTED_EDGE('',*,*,#2408,.F.);
#3377=ORIENTED_EDGE('',*,*,#2409,.F.);
#3378=ORIENTED_EDGE('',*,*,#2402,.T.);
#3379=ORIENTED_EDGE('',*,*,#2410,.F.);
#3380=ORIENTED_EDGE('',*,*,#2406,.T.);
#3381=ORIENTED_EDGE('',*,*,#2411,.F.);
#3382=ORIENTED_EDGE('',*,*,#2412,.T.);
#3383=ORIENTED_EDGE('',*,*,#2413,.T.);
#3384=ORIENTED_EDGE('',*,*,#2414,.F.);
#3385=ORIENTED_EDGE('',*,*,#2415,.T.);
#3386=ORIENTED_EDGE('',*,*,#2412,.F.);
#3387=ORIENTED_EDGE('',*,*,#2415,.F.);
#3388=ORIENTED_EDGE('',*,*,#2414,.T.);
#3389=ORIENTED_EDGE('',*,*,#2416,.F.);
#3390=ORIENTED_EDGE('',*,*,#2417,.T.);
#3391=ORIENTED_EDGE('',*,*,#2413,.F.);
#3392=ORIENTED_EDGE('',*,*,#2417,.F.);
#3393=ORIENTED_EDGE('',*,*,#2416,.T.);
#3394=ORIENTED_EDGE('',*,*,#2403,.T.);
#3395=ORIENTED_EDGE('',*,*,#2411,.T.);
#3396=ORIENTED_EDGE('',*,*,#2409,.T.);
#3397=ORIENTED_EDGE('',*,*,#2418,.F.);
#3398=ORIENTED_EDGE('',*,*,#2405,.T.);
#3399=ORIENTED_EDGE('',*,*,#2419,.F.);
#3400=ORIENTED_EDGE('',*,*,#2407,.T.);
#3401=ORIENTED_EDGE('',*,*,#2410,.T.);
#3402=ORIENTED_EDGE('',*,*,#2404,.T.);
#3403=ORIENTED_EDGE('',*,*,#2418,.T.);
#3404=ORIENTED_EDGE('',*,*,#2408,.T.);
#3405=ORIENTED_EDGE('',*,*,#2419,.T.);
#3406=ORIENTED_EDGE('',*,*,#2420,.F.);
#3407=ORIENTED_EDGE('',*,*,#2421,.F.);
#3408=ORIENTED_EDGE('',*,*,#2422,.F.);
#3409=ORIENTED_EDGE('',*,*,#2423,.F.);
#3410=ORIENTED_EDGE('',*,*,#2424,.F.);
#3411=ORIENTED_EDGE('',*,*,#2425,.F.);
#3412=ORIENTED_EDGE('',*,*,#2426,.F.);
#3413=ORIENTED_EDGE('',*,*,#2427,.F.);
#3414=ORIENTED_EDGE('',*,*,#2420,.T.);
#3415=ORIENTED_EDGE('',*,*,#2428,.F.);
#3416=ORIENTED_EDGE('',*,*,#2424,.T.);
#3417=ORIENTED_EDGE('',*,*,#2429,.F.);
#3418=ORIENTED_EDGE('',*,*,#2430,.T.);
#3419=ORIENTED_EDGE('',*,*,#2431,.T.);
#3420=ORIENTED_EDGE('',*,*,#2432,.F.);
#3421=ORIENTED_EDGE('',*,*,#2433,.T.);
#3422=ORIENTED_EDGE('',*,*,#2430,.F.);
#3423=ORIENTED_EDGE('',*,*,#2433,.F.);
#3424=ORIENTED_EDGE('',*,*,#2432,.T.);
#3425=ORIENTED_EDGE('',*,*,#2434,.F.);
#3426=ORIENTED_EDGE('',*,*,#2435,.T.);
#3427=ORIENTED_EDGE('',*,*,#2431,.F.);
#3428=ORIENTED_EDGE('',*,*,#2435,.F.);
#3429=ORIENTED_EDGE('',*,*,#2434,.T.);
#3430=ORIENTED_EDGE('',*,*,#2421,.T.);
#3431=ORIENTED_EDGE('',*,*,#2429,.T.);
#3432=ORIENTED_EDGE('',*,*,#2427,.T.);
#3433=ORIENTED_EDGE('',*,*,#2436,.F.);
#3434=ORIENTED_EDGE('',*,*,#2423,.T.);
#3435=ORIENTED_EDGE('',*,*,#2437,.F.);
#3436=ORIENTED_EDGE('',*,*,#2425,.T.);
#3437=ORIENTED_EDGE('',*,*,#2428,.T.);
#3438=ORIENTED_EDGE('',*,*,#2422,.T.);
#3439=ORIENTED_EDGE('',*,*,#2436,.T.);
#3440=ORIENTED_EDGE('',*,*,#2426,.T.);
#3441=ORIENTED_EDGE('',*,*,#2437,.T.);
#3442=ORIENTED_EDGE('',*,*,#2438,.F.);
#3443=ORIENTED_EDGE('',*,*,#2439,.F.);
#3444=ORIENTED_EDGE('',*,*,#2440,.F.);
#3445=ORIENTED_EDGE('',*,*,#2441,.F.);
#3446=ORIENTED_EDGE('',*,*,#2442,.F.);
#3447=ORIENTED_EDGE('',*,*,#2443,.F.);
#3448=ORIENTED_EDGE('',*,*,#2444,.F.);
#3449=ORIENTED_EDGE('',*,*,#2445,.F.);
#3450=ORIENTED_EDGE('',*,*,#2438,.T.);
#3451=ORIENTED_EDGE('',*,*,#2446,.F.);
#3452=ORIENTED_EDGE('',*,*,#2442,.T.);
#3453=ORIENTED_EDGE('',*,*,#2447,.F.);
#3454=ORIENTED_EDGE('',*,*,#2448,.T.);
#3455=ORIENTED_EDGE('',*,*,#2449,.T.);
#3456=ORIENTED_EDGE('',*,*,#2450,.F.);
#3457=ORIENTED_EDGE('',*,*,#2451,.T.);
#3458=ORIENTED_EDGE('',*,*,#2448,.F.);
#3459=ORIENTED_EDGE('',*,*,#2451,.F.);
#3460=ORIENTED_EDGE('',*,*,#2450,.T.);
#3461=ORIENTED_EDGE('',*,*,#2452,.F.);
#3462=ORIENTED_EDGE('',*,*,#2453,.T.);
#3463=ORIENTED_EDGE('',*,*,#2449,.F.);
#3464=ORIENTED_EDGE('',*,*,#2453,.F.);
#3465=ORIENTED_EDGE('',*,*,#2452,.T.);
#3466=ORIENTED_EDGE('',*,*,#2439,.T.);
#3467=ORIENTED_EDGE('',*,*,#2447,.T.);
#3468=ORIENTED_EDGE('',*,*,#2445,.T.);
#3469=ORIENTED_EDGE('',*,*,#2454,.F.);
#3470=ORIENTED_EDGE('',*,*,#2441,.T.);
#3471=ORIENTED_EDGE('',*,*,#2455,.F.);
#3472=ORIENTED_EDGE('',*,*,#2443,.T.);
#3473=ORIENTED_EDGE('',*,*,#2446,.T.);
#3474=ORIENTED_EDGE('',*,*,#2440,.T.);
#3475=ORIENTED_EDGE('',*,*,#2454,.T.);
#3476=ORIENTED_EDGE('',*,*,#2444,.T.);
#3477=ORIENTED_EDGE('',*,*,#2455,.T.);
#3478=CYLINDRICAL_SURFACE('',#3911,35.);
#3479=CYLINDRICAL_SURFACE('',#3925,33.);
#3480=CYLINDRICAL_SURFACE('',#3927,40.);
#3481=CYLINDRICAL_SURFACE('',#3934,1.25);
#3482=CYLINDRICAL_SURFACE('',#3938,0.75);
#3483=CYLINDRICAL_SURFACE('',#3949,1.1);
#3484=CYLINDRICAL_SURFACE('',#3952,1.1);
#3485=CYLINDRICAL_SURFACE('',#3955,4.99999999999999);
#3486=CYLINDRICAL_SURFACE('',#3957,33.8);
#3487=CYLINDRICAL_SURFACE('',#3966,34.);
#3488=CYLINDRICAL_SURFACE('',#3970,35.);
#3489=CYLINDRICAL_SURFACE('',#3975,1.1);
#3490=CYLINDRICAL_SURFACE('',#3978,1.1);
#3491=CYLINDRICAL_SURFACE('',#3981,25.);
#3492=CYLINDRICAL_SURFACE('',#3984,1.1);
#3493=CYLINDRICAL_SURFACE('',#3987,1.1);
#3494=CYLINDRICAL_SURFACE('',#3990,1.1);
#3495=CYLINDRICAL_SURFACE('',#3993,1.1);
#3496=CYLINDRICAL_SURFACE('',#3996,1.1);
#3497=CYLINDRICAL_SURFACE('',#3999,1.1);
#3498=CYLINDRICAL_SURFACE('',#4002,1.1);
#3499=CYLINDRICAL_SURFACE('',#4005,1.1);
#3500=CYLINDRICAL_SURFACE('',#4008,1.1);
#3501=CYLINDRICAL_SURFACE('',#4011,1.1);
#3502=CYLINDRICAL_SURFACE('',#4014,1.1);
#3503=CYLINDRICAL_SURFACE('',#4017,1.1);
#3504=CYLINDRICAL_SURFACE('',#4020,1.1);
#3505=CYLINDRICAL_SURFACE('',#4023,1.1);
#3506=CYLINDRICAL_SURFACE('',#4032,40.);
#3507=CYLINDRICAL_SURFACE('',#4044,6.);
#3508=CYLINDRICAL_SURFACE('',#4049,0.75);
#3509=CYLINDRICAL_SURFACE('',#4149,25.);
#3510=CYLINDRICAL_SURFACE('',#4214,34.);
#3511=CYLINDRICAL_SURFACE('',#4227,1.1);
#3512=CYLINDRICAL_SURFACE('',#4230,1.1);
#3513=CYLINDRICAL_SURFACE('',#4233,4.99999999999999);
#3514=CYLINDRICAL_SURFACE('',#4235,33.8);
#3515=CYLINDRICAL_SURFACE('',#4246,1.1);
#3516=CYLINDRICAL_SURFACE('',#4249,1.1);
#3517=CYLINDRICAL_SURFACE('',#4252,4.99999999999999);
#3518=CYLINDRICAL_SURFACE('',#4254,33.8);
#3519=CYLINDRICAL_SURFACE('',#4265,1.1);
#3520=CYLINDRICAL_SURFACE('',#4268,1.1);
#3521=CYLINDRICAL_SURFACE('',#4271,4.99999999999999);
#3522=CYLINDRICAL_SURFACE('',#4273,33.8);
#3523=CYLINDRICAL_SURFACE('',#4284,1.1);
#3524=CYLINDRICAL_SURFACE('',#4287,1.1);
#3525=CYLINDRICAL_SURFACE('',#4290,4.99999999999999);
#3526=CYLINDRICAL_SURFACE('',#4292,33.8);
#3527=CYLINDRICAL_SURFACE('',#4303,1.1);
#3528=CYLINDRICAL_SURFACE('',#4306,1.1);
#3529=CYLINDRICAL_SURFACE('',#4309,4.99999999999999);
#3530=CYLINDRICAL_SURFACE('',#4311,33.8);
#3531=CYLINDRICAL_SURFACE('',#4322,1.1);
#3532=CYLINDRICAL_SURFACE('',#4325,1.1);
#3533=CYLINDRICAL_SURFACE('',#4328,4.99999999999999);
#3534=CYLINDRICAL_SURFACE('',#4330,33.8);
#3535=CYLINDRICAL_SURFACE('',#4341,1.1);
#3536=CYLINDRICAL_SURFACE('',#4344,1.1);
#3537=CYLINDRICAL_SURFACE('',#4347,4.99999999999999);
#3538=CYLINDRICAL_SURFACE('',#4349,33.8);
#3539=ADVANCED_FACE('',(#333),#3478,.F.);
#3540=ADVANCED_FACE('',(#334,#129),#186,.F.);
#3541=ADVANCED_FACE('',(#335),#187,.F.);
#3542=ADVANCED_FACE('',(#336),#188,.F.);
#3543=ADVANCED_FACE('',(#337),#189,.F.);
#3544=ADVANCED_FACE('',(#338),#190,.F.);
#3545=ADVANCED_FACE('',(#339),#3479,.F.);
#3546=ADVANCED_FACE('',(#340),#3480,.T.);
#3547=ADVANCED_FACE('',(#341,#130),#191,.T.);
#3548=ADVANCED_FACE('',(#342),#74,.T.);
#3549=ADVANCED_FACE('',(#343),#3481,.T.);
#3550=ADVANCED_FACE('',(#344,#131),#192,.F.);
#3551=ADVANCED_FACE('',(#345),#3482,.T.);
#3552=ADVANCED_FACE('',(#346),#193,.F.);
#3553=ADVANCED_FACE('',(#347),#194,.F.);
#3554=ADVANCED_FACE('',(#348),#195,.F.);
#3555=ADVANCED_FACE('',(#349,#132,#133),#196,.F.);
#3556=ADVANCED_FACE('',(#350),#3483,.T.);
#3557=ADVANCED_FACE('',(#351),#197,.F.);
#3558=ADVANCED_FACE('',(#352),#3484,.T.);
#3559=ADVANCED_FACE('',(#353),#198,.F.);
#3560=ADVANCED_FACE('',(#354),#3485,.F.);
#3561=ADVANCED_FACE('',(#355),#3486,.T.);
#3562=ADVANCED_FACE('',(#356),#199,.T.);
#3563=ADVANCED_FACE('',(#357),#200,.F.);
#3564=ADVANCED_FACE('',(#358),#201,.F.);
#3565=ADVANCED_FACE('',(#359),#202,.F.);
#3566=ADVANCED_FACE('',(#360),#3487,.F.);
#3567=ADVANCED_FACE('',(#361,#134),#3488,.T.);
#3568=ADVANCED_FACE('',(#362,#135),#203,.F.);
#3569=ADVANCED_FACE('',(#363),#3489,.F.);
#3570=ADVANCED_FACE('',(#364),#3490,.F.);
#3571=ADVANCED_FACE('',(#365),#3491,.F.);
#3572=ADVANCED_FACE('',(#366),#3492,.F.);
#3573=ADVANCED_FACE('',(#367),#3493,.F.);
#3574=ADVANCED_FACE('',(#368),#3494,.F.);
#3575=ADVANCED_FACE('',(#369),#3495,.F.);
#3576=ADVANCED_FACE('',(#370),#3496,.F.);
#3577=ADVANCED_FACE('',(#371),#3497,.F.);
#3578=ADVANCED_FACE('',(#372),#3498,.F.);
#3579=ADVANCED_FACE('',(#373),#3499,.F.);
#3580=ADVANCED_FACE('',(#374),#3500,.F.);
#3581=ADVANCED_FACE('',(#375),#3501,.F.);
#3582=ADVANCED_FACE('',(#376),#3502,.F.);
#3583=ADVANCED_FACE('',(#377),#3503,.F.);
#3584=ADVANCED_FACE('',(#378),#3504,.F.);
#3585=ADVANCED_FACE('',(#379),#3505,.F.);
#3586=ADVANCED_FACE('',(#380,#136,#137,#138,#139,#140,#141,#142,#143,#144,
#145,#146,#147,#148,#149,#150,#151,#152),#204,.T.);
#3587=ADVANCED_FACE('',(#381,#153,#154,#155,#156,#157,#158,#159,#160,#161,
#162,#163,#164,#165,#166,#167,#168,#169),#205,.F.);
#3588=ADVANCED_FACE('',(#382),#206,.T.);
#3589=ADVANCED_FACE('',(#383),#3506,.F.);
#3590=ADVANCED_FACE('',(#384),#207,.F.);
#3591=ADVANCED_FACE('',(#385),#75,.F.);
#3592=ADVANCED_FACE('',(#386),#76,.F.);
#3593=ADVANCED_FACE('',(#387),#63,.T.);
#3594=ADVANCED_FACE('',(#388),#3507,.T.);
#3595=ADVANCED_FACE('',(#389),#208,.T.);
#3596=ADVANCED_FACE('',(#390),#64,.T.);
#3597=ADVANCED_FACE('',(#391),#3508,.F.);
#3598=ADVANCED_FACE('',(#392),#209,.T.);
#3599=ADVANCED_FACE('',(#393),#210,.F.);
#3600=ADVANCED_FACE('',(#394),#211,.F.);
#3601=ADVANCED_FACE('',(#395),#212,.F.);
#3602=ADVANCED_FACE('',(#396),#213,.F.);
#3603=ADVANCED_FACE('',(#397),#214,.F.);
#3604=ADVANCED_FACE('',(#398),#215,.F.);
#3605=ADVANCED_FACE('',(#399),#216,.F.);
#3606=ADVANCED_FACE('',(#400),#217,.F.);
#3607=ADVANCED_FACE('',(#401),#218,.F.);
#3608=ADVANCED_FACE('',(#402),#219,.F.);
#3609=ADVANCED_FACE('',(#403),#220,.F.);
#3610=ADVANCED_FACE('',(#404),#221,.F.);
#3611=ADVANCED_FACE('',(#405),#222,.F.);
#3612=ADVANCED_FACE('',(#406),#223,.F.);
#3613=ADVANCED_FACE('',(#407),#224,.F.);
#3614=ADVANCED_FACE('',(#408),#225,.F.);
#3615=ADVANCED_FACE('',(#409),#226,.F.);
#3616=ADVANCED_FACE('',(#410),#227,.F.);
#3617=ADVANCED_FACE('',(#411),#228,.F.);
#3618=ADVANCED_FACE('',(#412),#229,.T.);
#3619=ADVANCED_FACE('',(#413),#230,.T.);
#3620=ADVANCED_FACE('',(#414),#231,.T.);
#3621=ADVANCED_FACE('',(#415),#232,.T.);
#3622=ADVANCED_FACE('',(#416),#233,.T.);
#3623=ADVANCED_FACE('',(#417),#234,.T.);
#3624=ADVANCED_FACE('',(#418),#235,.T.);
#3625=ADVANCED_FACE('',(#419),#236,.T.);
#3626=ADVANCED_FACE('',(#420),#237,.T.);
#3627=ADVANCED_FACE('',(#421),#238,.T.);
#3628=ADVANCED_FACE('',(#422),#239,.T.);
#3629=ADVANCED_FACE('',(#423),#240,.T.);
#3630=ADVANCED_FACE('',(#424),#241,.T.);
#3631=ADVANCED_FACE('',(#425),#242,.T.);
#3632=ADVANCED_FACE('',(#426),#243,.T.);
#3633=ADVANCED_FACE('',(#427),#244,.T.);
#3634=ADVANCED_FACE('',(#428),#245,.T.);
#3635=ADVANCED_FACE('',(#429),#246,.T.);
#3636=ADVANCED_FACE('',(#430),#247,.T.);
#3637=ADVANCED_FACE('',(#431),#248,.F.);
#3638=ADVANCED_FACE('',(#432),#249,.F.);
#3639=ADVANCED_FACE('',(#433),#250,.F.);
#3640=ADVANCED_FACE('',(#434),#251,.F.);
#3641=ADVANCED_FACE('',(#435),#252,.F.);
#3642=ADVANCED_FACE('',(#436),#253,.F.);
#3643=ADVANCED_FACE('',(#437),#254,.F.);
#3644=ADVANCED_FACE('',(#438),#255,.F.);
#3645=ADVANCED_FACE('',(#439),#256,.F.);
#3646=ADVANCED_FACE('',(#440),#257,.F.);
#3647=ADVANCED_FACE('',(#441),#258,.F.);
#3648=ADVANCED_FACE('',(#442),#259,.F.);
#3649=ADVANCED_FACE('',(#443),#260,.F.);
#3650=ADVANCED_FACE('',(#444),#261,.F.);
#3651=ADVANCED_FACE('',(#445),#262,.F.);
#3652=ADVANCED_FACE('',(#446),#263,.F.);
#3653=ADVANCED_FACE('',(#447),#264,.F.);
#3654=ADVANCED_FACE('',(#448),#265,.F.);
#3655=ADVANCED_FACE('',(#449),#266,.F.);
#3656=ADVANCED_FACE('',(#450),#3509,.F.);
#3657=ADVANCED_FACE('',(#451),#267,.F.);
#3658=ADVANCED_FACE('',(#452),#268,.F.);
#3659=ADVANCED_FACE('',(#453),#269,.F.);
#3660=ADVANCED_FACE('',(#454),#270,.F.);
#3661=ADVANCED_FACE('',(#455),#271,.F.);
#3662=ADVANCED_FACE('',(#456),#272,.F.);
#3663=ADVANCED_FACE('',(#457),#273,.F.);
#3664=ADVANCED_FACE('',(#458),#274,.F.);
#3665=ADVANCED_FACE('',(#459),#275,.F.);
#3666=ADVANCED_FACE('',(#460),#276,.F.);
#3667=ADVANCED_FACE('',(#461),#277,.F.);
#3668=ADVANCED_FACE('',(#462),#278,.F.);
#3669=ADVANCED_FACE('',(#463),#279,.F.);
#3670=ADVANCED_FACE('',(#464),#280,.F.);
#3671=ADVANCED_FACE('',(#465),#281,.F.);
#3672=ADVANCED_FACE('',(#466),#282,.F.);
#3673=ADVANCED_FACE('',(#467),#283,.F.);
#3674=ADVANCED_FACE('',(#468),#284,.F.);
#3675=ADVANCED_FACE('',(#469),#285,.F.);
#3676=ADVANCED_FACE('',(#470),#286,.F.);
#3677=ADVANCED_FACE('',(#471),#287,.T.);
#3678=ADVANCED_FACE('',(#472),#288,.F.);
#3679=ADVANCED_FACE('',(#473,#170),#3510,.T.);
#3680=ADVANCED_FACE('',(#474,#171),#289,.T.);
#3681=ADVANCED_FACE('',(#475),#290,.F.);
#3682=ADVANCED_FACE('',(#476),#291,.F.);
#3683=ADVANCED_FACE('',(#477),#292,.F.);
#3684=ADVANCED_FACE('',(#478,#172,#173),#293,.F.);
#3685=ADVANCED_FACE('',(#479),#3511,.T.);
#3686=ADVANCED_FACE('',(#480),#294,.F.);
#3687=ADVANCED_FACE('',(#481),#3512,.T.);
#3688=ADVANCED_FACE('',(#482),#295,.F.);
#3689=ADVANCED_FACE('',(#483),#3513,.F.);
#3690=ADVANCED_FACE('',(#484),#3514,.T.);
#3691=ADVANCED_FACE('',(#485),#296,.T.);
#3692=ADVANCED_FACE('',(#486),#297,.F.);
#3693=ADVANCED_FACE('',(#487),#298,.F.);
#3694=ADVANCED_FACE('',(#488,#174,#175),#299,.F.);
#3695=ADVANCED_FACE('',(#489),#3515,.T.);
#3696=ADVANCED_FACE('',(#490),#300,.F.);
#3697=ADVANCED_FACE('',(#491),#3516,.T.);
#3698=ADVANCED_FACE('',(#492),#301,.F.);
#3699=ADVANCED_FACE('',(#493),#3517,.F.);
#3700=ADVANCED_FACE('',(#494),#3518,.T.);
#3701=ADVANCED_FACE('',(#495),#302,.T.);
#3702=ADVANCED_FACE('',(#496),#303,.F.);
#3703=ADVANCED_FACE('',(#497),#304,.F.);
#3704=ADVANCED_FACE('',(#498,#176,#177),#305,.F.);
#3705=ADVANCED_FACE('',(#499),#3519,.T.);
#3706=ADVANCED_FACE('',(#500),#306,.F.);
#3707=ADVANCED_FACE('',(#501),#3520,.T.);
#3708=ADVANCED_FACE('',(#502),#307,.F.);
#3709=ADVANCED_FACE('',(#503),#3521,.F.);
#3710=ADVANCED_FACE('',(#504),#3522,.T.);
#3711=ADVANCED_FACE('',(#505),#308,.T.);
#3712=ADVANCED_FACE('',(#506),#309,.F.);
#3713=ADVANCED_FACE('',(#507),#310,.F.);
#3714=ADVANCED_FACE('',(#508,#178,#179),#311,.F.);
#3715=ADVANCED_FACE('',(#509),#3523,.T.);
#3716=ADVANCED_FACE('',(#510),#312,.F.);
#3717=ADVANCED_FACE('',(#511),#3524,.T.);
#3718=ADVANCED_FACE('',(#512),#313,.F.);
#3719=ADVANCED_FACE('',(#513),#3525,.F.);
#3720=ADVANCED_FACE('',(#514),#3526,.T.);
#3721=ADVANCED_FACE('',(#515),#314,.T.);
#3722=ADVANCED_FACE('',(#516),#315,.F.);
#3723=ADVANCED_FACE('',(#517),#316,.F.);
#3724=ADVANCED_FACE('',(#518,#180,#181),#317,.F.);
#3725=ADVANCED_FACE('',(#519),#3527,.T.);
#3726=ADVANCED_FACE('',(#520),#318,.F.);
#3727=ADVANCED_FACE('',(#521),#3528,.T.);
#3728=ADVANCED_FACE('',(#522),#319,.F.);
#3729=ADVANCED_FACE('',(#523),#3529,.F.);
#3730=ADVANCED_FACE('',(#524),#3530,.T.);
#3731=ADVANCED_FACE('',(#525),#320,.T.);
#3732=ADVANCED_FACE('',(#526),#321,.F.);
#3733=ADVANCED_FACE('',(#527),#322,.F.);
#3734=ADVANCED_FACE('',(#528,#182,#183),#323,.F.);
#3735=ADVANCED_FACE('',(#529),#3531,.T.);
#3736=ADVANCED_FACE('',(#530),#324,.F.);
#3737=ADVANCED_FACE('',(#531),#3532,.T.);
#3738=ADVANCED_FACE('',(#532),#325,.F.);
#3739=ADVANCED_FACE('',(#533),#3533,.F.);
#3740=ADVANCED_FACE('',(#534),#3534,.T.);
#3741=ADVANCED_FACE('',(#535),#326,.T.);
#3742=ADVANCED_FACE('',(#536),#327,.F.);
#3743=ADVANCED_FACE('',(#537),#328,.F.);
#3744=ADVANCED_FACE('',(#538,#184,#185),#329,.F.);
#3745=ADVANCED_FACE('',(#539),#3535,.T.);
#3746=ADVANCED_FACE('',(#540),#330,.F.);
#3747=ADVANCED_FACE('',(#541),#3536,.T.);
#3748=ADVANCED_FACE('',(#542),#331,.F.);
#3749=ADVANCED_FACE('',(#543),#3537,.F.);
#3750=ADVANCED_FACE('',(#544),#3538,.T.);
#3751=ADVANCED_FACE('',(#545),#332,.T.);
#3752=CLOSED_SHELL('',(#3539,#3540,#3541,#3542,#3543,#3544,#3545,#3546,
#3547));
#3753=CLOSED_SHELL('',(#3548,#3549,#3550,#3551,#3552));
#3754=CLOSED_SHELL('',(#3553,#3554,#3555,#3556,#3557,#3558,#3559,#3560,
#3561,#3562));
#3755=CLOSED_SHELL('',(#3563,#3564,#3565,#3566,#3567,#3568,#3569,#3570,
#3571,#3572,#3573,#3574,#3575,#3576,#3577,#3578,#3579,#3580,#3581,#3582,
#3583,#3584,#3585,#3586,#3587));
#3756=CLOSED_SHELL('',(#3588,#3589,#3590,#3591,#3592,#3593,#3594,#3595,
#3596));
#3757=CLOSED_SHELL('',(#3597,#3598,#3599,#3600,#3601,#3602,#3603,#3604,
#3605,#3606,#3607,#3608,#3609,#3610,#3611,#3612,#3613,#3614,#3615,#3616,
#3617,#3618,#3619,#3620,#3621,#3622,#3623,#3624,#3625,#3626,#3627,#3628,
#3629,#3630,#3631,#3632,#3633,#3634,#3635,#3636,#3637,#3638,#3639,#3640,
#3641,#3642,#3643,#3644,#3645,#3646,#3647,#3648,#3649,#3650,#3651,#3652,
#3653,#3654,#3655,#3656,#3657,#3658,#3659,#3660,#3661,#3662,#3663,#3664,
#3665,#3666,#3667,#3668,#3669,#3670,#3671,#3672,#3673,#3674,#3675,#3676,
#3677,#3678,#3679,#3680,#3681));
#3758=CLOSED_SHELL('',(#3682,#3683,#3684,#3685,#3686,#3687,#3688,#3689,
#3690,#3691));
#3759=CLOSED_SHELL('',(#3692,#3693,#3694,#3695,#3696,#3697,#3698,#3699,
#3700,#3701));
#3760=CLOSED_SHELL('',(#3702,#3703,#3704,#3705,#3706,#3707,#3708,#3709,
#3710,#3711));
#3761=CLOSED_SHELL('',(#3712,#3713,#3714,#3715,#3716,#3717,#3718,#3719,
#3720,#3721));
#3762=CLOSED_SHELL('',(#3722,#3723,#3724,#3725,#3726,#3727,#3728,#3729,
#3730,#3731));
#3763=CLOSED_SHELL('',(#3732,#3733,#3734,#3735,#3736,#3737,#3738,#3739,
#3740,#3741));
#3764=CLOSED_SHELL('',(#3742,#3743,#3744,#3745,#3746,#3747,#3748,#3749,
#3750,#3751));
#3765=DERIVED_UNIT_ELEMENT(#3791,1.);
#3766=DERIVED_UNIT_ELEMENT(#6755,-3.);
#3767=DERIVED_UNIT_ELEMENT(#3791,1.);
#3768=DERIVED_UNIT_ELEMENT(#6755,-3.);
#3769=DERIVED_UNIT_ELEMENT(#3791,1.);
#3770=DERIVED_UNIT_ELEMENT(#6755,-3.);
#3771=DERIVED_UNIT_ELEMENT(#3791,1.);
#3772=DERIVED_UNIT_ELEMENT(#6755,-3.);
#3773=DERIVED_UNIT_ELEMENT(#3791,1.);
#3774=DERIVED_UNIT_ELEMENT(#6755,-3.);
#3775=DERIVED_UNIT_ELEMENT(#3791,1.);
#3776=DERIVED_UNIT_ELEMENT(#6755,-3.);
#3777=DERIVED_UNIT_ELEMENT(#3791,1.);
#3778=DERIVED_UNIT_ELEMENT(#6755,-3.);
#3779=DERIVED_UNIT_ELEMENT(#3791,1.);
#3780=DERIVED_UNIT_ELEMENT(#6755,-3.);
#3781=DERIVED_UNIT_ELEMENT(#3791,1.);
#3782=DERIVED_UNIT_ELEMENT(#6755,-3.);
#3783=DERIVED_UNIT_ELEMENT(#3791,1.);
#3784=DERIVED_UNIT_ELEMENT(#6755,-3.);
#3785=DERIVED_UNIT_ELEMENT(#3791,1.);
#3786=DERIVED_UNIT_ELEMENT(#6755,-3.);
#3787=DERIVED_UNIT_ELEMENT(#3791,1.);
#3788=DERIVED_UNIT_ELEMENT(#6755,-3.);
#3789=DERIVED_UNIT_ELEMENT(#3791,1.);
#3790=DERIVED_UNIT_ELEMENT(#6755,-3.);
#3791=(
MASS_UNIT()
NAMED_UNIT(*)
SI_UNIT(.KILO.,.GRAM.)
);
#3792=DERIVED_UNIT((#3765,#3766));
#3793=DERIVED_UNIT((#3767,#3768));
#3794=DERIVED_UNIT((#3769,#3770));
#3795=DERIVED_UNIT((#3771,#3772));
#3796=DERIVED_UNIT((#3773,#3774));
#3797=DERIVED_UNIT((#3775,#3776));
#3798=DERIVED_UNIT((#3777,#3778));
#3799=DERIVED_UNIT((#3779,#3780));
#3800=DERIVED_UNIT((#3781,#3782));
#3801=DERIVED_UNIT((#3783,#3784));
#3802=DERIVED_UNIT((#3785,#3786));
#3803=DERIVED_UNIT((#3787,#3788));
#3804=DERIVED_UNIT((#3789,#3790));
#3805=MEASURE_REPRESENTATION_ITEM('density measure',
POSITIVE_RATIO_MEASURE(7850.),#3792);
#3806=MEASURE_REPRESENTATION_ITEM('density measure',
POSITIVE_RATIO_MEASURE(7850.),#3793);
#3807=MEASURE_REPRESENTATION_ITEM('density measure',
POSITIVE_RATIO_MEASURE(7850.),#3794);
#3808=MEASURE_REPRESENTATION_ITEM('density measure',
POSITIVE_RATIO_MEASURE(7850.),#3795);
#3809=MEASURE_REPRESENTATION_ITEM('density measure',
POSITIVE_RATIO_MEASURE(7850.),#3796);
#3810=MEASURE_REPRESENTATION_ITEM('density measure',
POSITIVE_RATIO_MEASURE(7850.),#3797);
#3811=MEASURE_REPRESENTATION_ITEM('density measure',
POSITIVE_RATIO_MEASURE(7850.),#3798);
#3812=MEASURE_REPRESENTATION_ITEM('density measure',
POSITIVE_RATIO_MEASURE(7850.),#3799);
#3813=MEASURE_REPRESENTATION_ITEM('density measure',
POSITIVE_RATIO_MEASURE(7850.),#3800);
#3814=MEASURE_REPRESENTATION_ITEM('density measure',
POSITIVE_RATIO_MEASURE(7850.),#3801);
#3815=MEASURE_REPRESENTATION_ITEM('density measure',
POSITIVE_RATIO_MEASURE(7850.),#3802);
#3816=MEASURE_REPRESENTATION_ITEM('density measure',
POSITIVE_RATIO_MEASURE(7850.),#3803);
#3817=MEASURE_REPRESENTATION_ITEM('density measure',
POSITIVE_RATIO_MEASURE(7850.),#3804);
#3818=PROPERTY_DEFINITION_REPRESENTATION(#3883,#3844);
#3819=PROPERTY_DEFINITION_REPRESENTATION(#3884,#3845);
#3820=PROPERTY_DEFINITION_REPRESENTATION(#3885,#3846);
#3821=PROPERTY_DEFINITION_REPRESENTATION(#3886,#3847);
#3822=PROPERTY_DEFINITION_REPRESENTATION(#3887,#3848);
#3823=PROPERTY_DEFINITION_REPRESENTATION(#3888,#3849);
#3824=PROPERTY_DEFINITION_REPRESENTATION(#3889,#3850);
#3825=PROPERTY_DEFINITION_REPRESENTATION(#3890,#3851);
#3826=PROPERTY_DEFINITION_REPRESENTATION(#3891,#3852);
#3827=PROPERTY_DEFINITION_REPRESENTATION(#3892,#3853);
#3828=PROPERTY_DEFINITION_REPRESENTATION(#3893,#3854);
#3829=PROPERTY_DEFINITION_REPRESENTATION(#3894,#3855);
#3830=PROPERTY_DEFINITION_REPRESENTATION(#3895,#3856);
#3831=PROPERTY_DEFINITION_REPRESENTATION(#3896,#3857);
#3832=PROPERTY_DEFINITION_REPRESENTATION(#3897,#3858);
#3833=PROPERTY_DEFINITION_REPRESENTATION(#3898,#3859);
#3834=PROPERTY_DEFINITION_REPRESENTATION(#3899,#3860);
#3835=PROPERTY_DEFINITION_REPRESENTATION(#3900,#3861);
#3836=PROPERTY_DEFINITION_REPRESENTATION(#3901,#3862);
#3837=PROPERTY_DEFINITION_REPRESENTATION(#3902,#3863);
#3838=PROPERTY_DEFINITION_REPRESENTATION(#3903,#3864);
#3839=PROPERTY_DEFINITION_REPRESENTATION(#3904,#3865);
#3840=PROPERTY_DEFINITION_REPRESENTATION(#3905,#3866);
#3841=PROPERTY_DEFINITION_REPRESENTATION(#3906,#3867);
#3842=PROPERTY_DEFINITION_REPRESENTATION(#3907,#3868);
#3843=PROPERTY_DEFINITION_REPRESENTATION(#3908,#3869);
#3844=REPRESENTATION('material name',(#3870),#6740);
#3845=REPRESENTATION('density',(#3805),#6740);
#3846=REPRESENTATION('material name',(#3871),#6741);
#3847=REPRESENTATION('density',(#3806),#6741);
#3848=REPRESENTATION('material name',(#3872),#6742);
#3849=REPRESENTATION('density',(#3807),#6742);
#3850=REPRESENTATION('material name',(#3873),#6743);
#3851=REPRESENTATION('density',(#3808),#6743);
#3852=REPRESENTATION('material name',(#3874),#6744);
#3853=REPRESENTATION('density',(#3809),#6744);
#3854=REPRESENTATION('material name',(#3875),#6745);
#3855=REPRESENTATION('density',(#3810),#6745);
#3856=REPRESENTATION('material name',(#3876),#6746);
#3857=REPRESENTATION('density',(#3811),#6746);
#3858=REPRESENTATION('material name',(#3877),#6747);
#3859=REPRESENTATION('density',(#3812),#6747);
#3860=REPRESENTATION('material name',(#3878),#6748);
#3861=REPRESENTATION('density',(#3813),#6748);
#3862=REPRESENTATION('material name',(#3879),#6749);
#3863=REPRESENTATION('density',(#3814),#6749);
#3864=REPRESENTATION('material name',(#3880),#6750);
#3865=REPRESENTATION('density',(#3815),#6750);
#3866=REPRESENTATION('material name',(#3881),#6751);
#3867=REPRESENTATION('density',(#3816),#6751);
#3868=REPRESENTATION('material name',(#3882),#6752);
#3869=REPRESENTATION('density',(#3817),#6752);
#3870=DESCRIPTIVE_REPRESENTATION_ITEM('Steel','Steel');
#3871=DESCRIPTIVE_REPRESENTATION_ITEM('Steel','Steel');
#3872=DESCRIPTIVE_REPRESENTATION_ITEM('Steel','Steel');
#3873=DESCRIPTIVE_REPRESENTATION_ITEM('Steel','Steel');
#3874=DESCRIPTIVE_REPRESENTATION_ITEM('Steel','Steel');
#3875=DESCRIPTIVE_REPRESENTATION_ITEM('Steel','Steel');
#3876=DESCRIPTIVE_REPRESENTATION_ITEM('Steel','Steel');
#3877=DESCRIPTIVE_REPRESENTATION_ITEM('Steel','Steel');
#3878=DESCRIPTIVE_REPRESENTATION_ITEM('Steel','Steel');
#3879=DESCRIPTIVE_REPRESENTATION_ITEM('Steel','Steel');
#3880=DESCRIPTIVE_REPRESENTATION_ITEM('Steel','Steel');
#3881=DESCRIPTIVE_REPRESENTATION_ITEM('Steel','Steel');
#3882=DESCRIPTIVE_REPRESENTATION_ITEM('Steel','Steel');
#3883=PROPERTY_DEFINITION('material property','material name',#6815);
#3884=PROPERTY_DEFINITION('material property','density of part',#6815);
#3885=PROPERTY_DEFINITION('material property','material name',#6816);
#3886=PROPERTY_DEFINITION('material property','density of part',#6816);
#3887=PROPERTY_DEFINITION('material property','material name',#6817);
#3888=PROPERTY_DEFINITION('material property','density of part',#6817);
#3889=PROPERTY_DEFINITION('material property','material name',#6818);
#3890=PROPERTY_DEFINITION('material property','density of part',#6818);
#3891=PROPERTY_DEFINITION('material property','material name',#6819);
#3892=PROPERTY_DEFINITION('material property','density of part',#6819);
#3893=PROPERTY_DEFINITION('material property','material name',#6820);
#3894=PROPERTY_DEFINITION('material property','density of part',#6820);
#3895=PROPERTY_DEFINITION('material property','material name',#6821);
#3896=PROPERTY_DEFINITION('material property','density of part',#6821);
#3897=PROPERTY_DEFINITION('material property','material name',#6822);
#3898=PROPERTY_DEFINITION('material property','density of part',#6822);
#3899=PROPERTY_DEFINITION('material property','material name',#6823);
#3900=PROPERTY_DEFINITION('material property','density of part',#6823);
#3901=PROPERTY_DEFINITION('material property','material name',#6824);
#3902=PROPERTY_DEFINITION('material property','density of part',#6824);
#3903=PROPERTY_DEFINITION('material property','material name',#6825);
#3904=PROPERTY_DEFINITION('material property','density of part',#6825);
#3905=PROPERTY_DEFINITION('material property','material name',#6826);
#3906=PROPERTY_DEFINITION('material property','density of part',#6826);
#3907=PROPERTY_DEFINITION('material property','material name',#6827);
#3908=PROPERTY_DEFINITION('material property','density of part',#6827);
#3909=AXIS2_PLACEMENT_3D('',#5563,#4365,#4366);
#3910=AXIS2_PLACEMENT_3D('',#5564,#4367,#4368);
#3911=AXIS2_PLACEMENT_3D('',#5565,#4369,#4370);
#3912=AXIS2_PLACEMENT_3D('',#5570,#4372,#4373);
#3913=AXIS2_PLACEMENT_3D('',#5573,#4375,#4376);
#3914=AXIS2_PLACEMENT_3D('',#5575,#4377,#4378);
#3915=AXIS2_PLACEMENT_3D('',#5578,#4380,#4381);
#3916=AXIS2_PLACEMENT_3D('',#5579,#4382,#4383);
#3917=AXIS2_PLACEMENT_3D('',#5581,#4384,#4385);
#3918=AXIS2_PLACEMENT_3D('',#5582,#4386,#4387);
#3919=AXIS2_PLACEMENT_3D('',#5586,#4389,#4390);
#3920=AXIS2_PLACEMENT_3D('',#5588,#4391,#4392);
#3921=AXIS2_PLACEMENT_3D('',#5590,#4394,#4395);
#3922=AXIS2_PLACEMENT_3D('',#5594,#4398,#4399);
#3923=AXIS2_PLACEMENT_3D('',#5598,#4402,#4403);
#3924=AXIS2_PLACEMENT_3D('',#5599,#4404,#4405);
#3925=AXIS2_PLACEMENT_3D('',#5600,#4406,#4407);
#3926=AXIS2_PLACEMENT_3D('',#5602,#4408,#4409);
#3927=AXIS2_PLACEMENT_3D('',#5604,#4411,#4412);
#3928=AXIS2_PLACEMENT_3D('',#5606,#4413,#4414);
#3929=AXIS2_PLACEMENT_3D('',#5608,#4416,#4417);
#3930=AXIS2_PLACEMENT_3D('',#5609,#4418,#4419);
#3931=AXIS2_PLACEMENT_3D('',#5610,#4420,#4421);
#3932=AXIS2_PLACEMENT_3D('',#5612,#4422,#4423);
#3933=AXIS2_PLACEMENT_3D('',#5614,#4424,#4425);
#3934=AXIS2_PLACEMENT_3D('',#5615,#4426,#4427);
#3935=AXIS2_PLACEMENT_3D('',#5618,#4429,#4430);
#3936=AXIS2_PLACEMENT_3D('',#5619,#4431,#4432);
#3937=AXIS2_PLACEMENT_3D('',#5621,#4433,#4434);
#3938=AXIS2_PLACEMENT_3D('',#5622,#4435,#4436);
#3939=AXIS2_PLACEMENT_3D('',#5624,#4437,#4438);
#3940=AXIS2_PLACEMENT_3D('',#5626,#4440,#4441);
#3941=AXIS2_PLACEMENT_3D('',#5627,#4442,#4443);
#3942=AXIS2_PLACEMENT_3D('',#5628,#4444,#4445);
#3943=AXIS2_PLACEMENT_3D('',#5637,#4450,#4451);
#3944=AXIS2_PLACEMENT_3D('',#5646,#4456,#4457);
#3945=AXIS2_PLACEMENT_3D('',#5647,#4458,#4459);
#3946=AXIS2_PLACEMENT_3D('',#5648,#4460,#4461);
#3947=AXIS2_PLACEMENT_3D('',#5650,#4462,#4463);
#3948=AXIS2_PLACEMENT_3D('',#5652,#4464,#4465);
#3949=AXIS2_PLACEMENT_3D('',#5653,#4466,#4467);
#3950=AXIS2_PLACEMENT_3D('',#5655,#4468,#4469);
#3951=AXIS2_PLACEMENT_3D('',#5657,#4471,#4472);
#3952=AXIS2_PLACEMENT_3D('',#5658,#4473,#4474);
#3953=AXIS2_PLACEMENT_3D('',#5660,#4475,#4476);
#3954=AXIS2_PLACEMENT_3D('',#5662,#4478,#4479);
#3955=AXIS2_PLACEMENT_3D('',#5663,#4480,#4481);
#3956=AXIS2_PLACEMENT_3D('',#5664,#4482,#4483);
#3957=AXIS2_PLACEMENT_3D('',#5665,#4484,#4485);
#3958=AXIS2_PLACEMENT_3D('',#5666,#4486,#4487);
#3959=AXIS2_PLACEMENT_3D('',#5667,#4488,#4489);
#3960=AXIS2_PLACEMENT_3D('',#5668,#4490,#4491);
#3961=AXIS2_PLACEMENT_3D('',#5669,#4492,#4493);
#3962=AXIS2_PLACEMENT_3D('',#5672,#4494,#4495);
#3963=AXIS2_PLACEMENT_3D('',#5676,#4497,#4498);
#3964=AXIS2_PLACEMENT_3D('',#5678,#4500,#4501);
#3965=AXIS2_PLACEMENT_3D('',#5684,#4505,#4506);
#3966=AXIS2_PLACEMENT_3D('',#5690,#4510,#4511);
#3967=AXIS2_PLACEMENT_3D('',#5692,#4512,#4513);
#3968=AXIS2_PLACEMENT_3D('',#5695,#4515,#4516);
#3969=AXIS2_PLACEMENT_3D('',#5696,#4517,#4518);
#3970=AXIS2_PLACEMENT_3D('',#5697,#4519,#4520);
#3971=AXIS2_PLACEMENT_3D('',#5699,#4521,#4522);
#3972=AXIS2_PLACEMENT_3D('',#5702,#4524,#4525);
#3973=AXIS2_PLACEMENT_3D('',#5703,#4526,#4527);
#3974=AXIS2_PLACEMENT_3D('',#5704,#4528,#4529);
#3975=AXIS2_PLACEMENT_3D('',#5705,#4530,#4531);
#3976=AXIS2_PLACEMENT_3D('',#5707,#4532,#4533);
#3977=AXIS2_PLACEMENT_3D('',#5710,#4535,#4536);
#3978=AXIS2_PLACEMENT_3D('',#5711,#4537,#4538);
#3979=AXIS2_PLACEMENT_3D('',#5713,#4539,#4540);
#3980=AXIS2_PLACEMENT_3D('',#5716,#4542,#4543);
#3981=AXIS2_PLACEMENT_3D('',#5717,#4544,#4545);
#3982=AXIS2_PLACEMENT_3D('',#5719,#4546,#4547);
#3983=AXIS2_PLACEMENT_3D('',#5722,#4549,#4550);
#3984=AXIS2_PLACEMENT_3D('',#5723,#4551,#4552);
#3985=AXIS2_PLACEMENT_3D('',#5725,#4553,#4554);
#3986=AXIS2_PLACEMENT_3D('',#5728,#4556,#4557);
#3987=AXIS2_PLACEMENT_3D('',#5729,#4558,#4559);
#3988=AXIS2_PLACEMENT_3D('',#5731,#4560,#4561);
#3989=AXIS2_PLACEMENT_3D('',#5734,#4563,#4564);
#3990=AXIS2_PLACEMENT_3D('',#5735,#4565,#4566);
#3991=AXIS2_PLACEMENT_3D('',#5737,#4567,#4568);
#3992=AXIS2_PLACEMENT_3D('',#5740,#4570,#4571);
#3993=AXIS2_PLACEMENT_3D('',#5741,#4572,#4573);
#3994=AXIS2_PLACEMENT_3D('',#5743,#4574,#4575);
#3995=AXIS2_PLACEMENT_3D('',#5746,#4577,#4578);
#3996=AXIS2_PLACEMENT_3D('',#5747,#4579,#4580);
#3997=AXIS2_PLACEMENT_3D('',#5749,#4581,#4582);
#3998=AXIS2_PLACEMENT_3D('',#5752,#4584,#4585);
#3999=AXIS2_PLACEMENT_3D('',#5753,#4586,#4587);
#4000=AXIS2_PLACEMENT_3D('',#5755,#4588,#4589);
#4001=AXIS2_PLACEMENT_3D('',#5758,#4591,#4592);
#4002=AXIS2_PLACEMENT_3D('',#5759,#4593,#4594);
#4003=AXIS2_PLACEMENT_3D('',#5761,#4595,#4596);
#4004=AXIS2_PLACEMENT_3D('',#5764,#4598,#4599);
#4005=AXIS2_PLACEMENT_3D('',#5765,#4600,#4601);
#4006=AXIS2_PLACEMENT_3D('',#5767,#4602,#4603);
#4007=AXIS2_PLACEMENT_3D('',#5770,#4605,#4606);
#4008=AXIS2_PLACEMENT_3D('',#5771,#4607,#4608);
#4009=AXIS2_PLACEMENT_3D('',#5773,#4609,#4610);
#4010=AXIS2_PLACEMENT_3D('',#5776,#4612,#4613);
#4011=AXIS2_PLACEMENT_3D('',#5777,#4614,#4615);
#4012=AXIS2_PLACEMENT_3D('',#5779,#4616,#4617);
#4013=AXIS2_PLACEMENT_3D('',#5782,#4619,#4620);
#4014=AXIS2_PLACEMENT_3D('',#5783,#4621,#4622);
#4015=AXIS2_PLACEMENT_3D('',#5785,#4623,#4624);
#4016=AXIS2_PLACEMENT_3D('',#5788,#4626,#4627);
#4017=AXIS2_PLACEMENT_3D('',#5789,#4628,#4629);
#4018=AXIS2_PLACEMENT_3D('',#5791,#4630,#4631);
#4019=AXIS2_PLACEMENT_3D('',#5794,#4633,#4634);
#4020=AXIS2_PLACEMENT_3D('',#5795,#4635,#4636);
#4021=AXIS2_PLACEMENT_3D('',#5797,#4637,#4638);
#4022=AXIS2_PLACEMENT_3D('',#5800,#4640,#4641);
#4023=AXIS2_PLACEMENT_3D('',#5801,#4642,#4643);
#4024=AXIS2_PLACEMENT_3D('',#5803,#4644,#4645);
#4025=AXIS2_PLACEMENT_3D('',#5806,#4647,#4648);
#4026=AXIS2_PLACEMENT_3D('',#5807,#4649,#4650);
#4027=AXIS2_PLACEMENT_3D('',#5808,#4651,#4652);
#4028=AXIS2_PLACEMENT_3D('',#5809,#4653,#4654);
#4029=AXIS2_PLACEMENT_3D('',#5810,#4655,#4656);
#4030=AXIS2_PLACEMENT_3D('',#5817,#4657,#4658);
#4031=AXIS2_PLACEMENT_3D('',#5822,#4659,#4660);
#4032=AXIS2_PLACEMENT_3D('',#5823,#4661,#4662);
#4033=AXIS2_PLACEMENT_3D('',#5835,#4663,#4664);
#4034=AXIS2_PLACEMENT_3D('',#5861,#4665,#4666);
#4035=AXIS2_PLACEMENT_3D('',#5867,#4667,#4668);
#4036=AXIS2_PLACEMENT_3D('',#5871,#4669,#4670);
#4037=AXIS2_PLACEMENT_3D('',#5872,#4671,#4672);
#4038=AXIS2_PLACEMENT_3D('',#5873,#4673,#4674);
#4039=AXIS2_PLACEMENT_3D('',#5874,#4675,#4676);
#4040=AXIS2_PLACEMENT_3D('',#5875,#4677,#4678);
#4041=AXIS2_PLACEMENT_3D('',#5877,#4679,#4680);
#4042=AXIS2_PLACEMENT_3D('',#5881,#4682,#4683);
#4043=AXIS2_PLACEMENT_3D('',#5882,#4684,#4685);
#4044=AXIS2_PLACEMENT_3D('',#5883,#4686,#4687);
#4045=AXIS2_PLACEMENT_3D('',#5886,#4689,#4690);
#4046=AXIS2_PLACEMENT_3D('',#5887,#4691,#4692);
#4047=AXIS2_PLACEMENT_3D('',#5888,#4693,#4694);
#4048=AXIS2_PLACEMENT_3D('',#5890,#4696,#4697);
#4049=AXIS2_PLACEMENT_3D('',#5891,#4698,#4699);
#4050=AXIS2_PLACEMENT_3D('',#5929,#4701,#4702);
#4051=AXIS2_PLACEMENT_3D('',#5930,#4703,#4704);
#4052=AXIS2_PLACEMENT_3D('',#5931,#4705,#4706);
#4053=AXIS2_PLACEMENT_3D('',#5940,#4711,#4712);
#4054=AXIS2_PLACEMENT_3D('',#5949,#4717,#4718);
#4055=AXIS2_PLACEMENT_3D('',#5958,#4723,#4724);
#4056=AXIS2_PLACEMENT_3D('',#5967,#4729,#4730);
#4057=AXIS2_PLACEMENT_3D('',#5976,#4735,#4736);
#4058=AXIS2_PLACEMENT_3D('',#5985,#4741,#4742);
#4059=AXIS2_PLACEMENT_3D('',#5994,#4747,#4748);
#4060=AXIS2_PLACEMENT_3D('',#6003,#4753,#4754);
#4061=AXIS2_PLACEMENT_3D('',#6012,#4759,#4760);
#4062=AXIS2_PLACEMENT_3D('',#6021,#4765,#4766);
#4063=AXIS2_PLACEMENT_3D('',#6030,#4771,#4772);
#4064=AXIS2_PLACEMENT_3D('',#6039,#4777,#4778);
#4065=AXIS2_PLACEMENT_3D('',#6048,#4783,#4784);
#4066=AXIS2_PLACEMENT_3D('',#6057,#4789,#4790);
#4067=AXIS2_PLACEMENT_3D('',#6066,#4795,#4796);
#4068=AXIS2_PLACEMENT_3D('',#6075,#4801,#4802);
#4069=AXIS2_PLACEMENT_3D('',#6084,#4807,#4808);
#4070=AXIS2_PLACEMENT_3D('',#6093,#4813,#4814);
#4071=AXIS2_PLACEMENT_3D('',#6102,#4819,#4820);
#4072=AXIS2_PLACEMENT_3D('',#6105,#4821,#4822);
#4073=AXIS2_PLACEMENT_3D('',#6109,#4824,#4825);
#4074=AXIS2_PLACEMENT_3D('',#6110,#4826,#4827);
#4075=AXIS2_PLACEMENT_3D('',#6111,#4828,#4829);
#4076=AXIS2_PLACEMENT_3D('',#6112,#4830,#4831);
#4077=AXIS2_PLACEMENT_3D('',#6114,#4832,#4833);
#4078=AXIS2_PLACEMENT_3D('',#6117,#4835,#4836);
#4079=AXIS2_PLACEMENT_3D('',#6118,#4837,#4838);
#4080=AXIS2_PLACEMENT_3D('',#6120,#4839,#4840);
#4081=AXIS2_PLACEMENT_3D('',#6123,#4842,#4843);
#4082=AXIS2_PLACEMENT_3D('',#6124,#4844,#4845);
#4083=AXIS2_PLACEMENT_3D('',#6126,#4846,#4847);
#4084=AXIS2_PLACEMENT_3D('',#6129,#4849,#4850);
#4085=AXIS2_PLACEMENT_3D('',#6130,#4851,#4852);
#4086=AXIS2_PLACEMENT_3D('',#6132,#4853,#4854);
#4087=AXIS2_PLACEMENT_3D('',#6135,#4856,#4857);
#4088=AXIS2_PLACEMENT_3D('',#6136,#4858,#4859);
#4089=AXIS2_PLACEMENT_3D('',#6138,#4860,#4861);
#4090=AXIS2_PLACEMENT_3D('',#6141,#4863,#4864);
#4091=AXIS2_PLACEMENT_3D('',#6142,#4865,#4866);
#4092=AXIS2_PLACEMENT_3D('',#6144,#4867,#4868);
#4093=AXIS2_PLACEMENT_3D('',#6147,#4870,#4871);
#4094=AXIS2_PLACEMENT_3D('',#6148,#4872,#4873);
#4095=AXIS2_PLACEMENT_3D('',#6150,#4874,#4875);
#4096=AXIS2_PLACEMENT_3D('',#6153,#4877,#4878);
#4097=AXIS2_PLACEMENT_3D('',#6154,#4879,#4880);
#4098=AXIS2_PLACEMENT_3D('',#6156,#4881,#4882);
#4099=AXIS2_PLACEMENT_3D('',#6159,#4884,#4885);
#4100=AXIS2_PLACEMENT_3D('',#6160,#4886,#4887);
#4101=AXIS2_PLACEMENT_3D('',#6162,#4888,#4889);
#4102=AXIS2_PLACEMENT_3D('',#6165,#4891,#4892);
#4103=AXIS2_PLACEMENT_3D('',#6166,#4893,#4894);
#4104=AXIS2_PLACEMENT_3D('',#6168,#4895,#4896);
#4105=AXIS2_PLACEMENT_3D('',#6171,#4898,#4899);
#4106=AXIS2_PLACEMENT_3D('',#6172,#4900,#4901);
#4107=AXIS2_PLACEMENT_3D('',#6174,#4902,#4903);
#4108=AXIS2_PLACEMENT_3D('',#6177,#4905,#4906);
#4109=AXIS2_PLACEMENT_3D('',#6178,#4907,#4908);
#4110=AXIS2_PLACEMENT_3D('',#6180,#4909,#4910);
#4111=AXIS2_PLACEMENT_3D('',#6183,#4912,#4913);
#4112=AXIS2_PLACEMENT_3D('',#6184,#4914,#4915);
#4113=AXIS2_PLACEMENT_3D('',#6186,#4916,#4917);
#4114=AXIS2_PLACEMENT_3D('',#6189,#4919,#4920);
#4115=AXIS2_PLACEMENT_3D('',#6190,#4921,#4922);
#4116=AXIS2_PLACEMENT_3D('',#6192,#4923,#4924);
#4117=AXIS2_PLACEMENT_3D('',#6195,#4926,#4927);
#4118=AXIS2_PLACEMENT_3D('',#6196,#4928,#4929);
#4119=AXIS2_PLACEMENT_3D('',#6198,#4930,#4931);
#4120=AXIS2_PLACEMENT_3D('',#6201,#4933,#4934);
#4121=AXIS2_PLACEMENT_3D('',#6202,#4935,#4936);
#4122=AXIS2_PLACEMENT_3D('',#6204,#4937,#4938);
#4123=AXIS2_PLACEMENT_3D('',#6207,#4940,#4941);
#4124=AXIS2_PLACEMENT_3D('',#6208,#4942,#4943);
#4125=AXIS2_PLACEMENT_3D('',#6210,#4944,#4945);
#4126=AXIS2_PLACEMENT_3D('',#6213,#4947,#4948);
#4127=AXIS2_PLACEMENT_3D('',#6214,#4949,#4950);
#4128=AXIS2_PLACEMENT_3D('',#6216,#4951,#4952);
#4129=AXIS2_PLACEMENT_3D('',#6219,#4954,#4955);
#4130=AXIS2_PLACEMENT_3D('',#6220,#4956,#4957);
#4131=AXIS2_PLACEMENT_3D('',#6226,#4961,#4962);
#4132=AXIS2_PLACEMENT_3D('',#6232,#4966,#4967);
#4133=AXIS2_PLACEMENT_3D('',#6238,#4971,#4972);
#4134=AXIS2_PLACEMENT_3D('',#6244,#4976,#4977);
#4135=AXIS2_PLACEMENT_3D('',#6250,#4981,#4982);
#4136=AXIS2_PLACEMENT_3D('',#6256,#4986,#4987);
#4137=AXIS2_PLACEMENT_3D('',#6262,#4991,#4992);
#4138=AXIS2_PLACEMENT_3D('',#6268,#4996,#4997);
#4139=AXIS2_PLACEMENT_3D('',#6274,#5001,#5002);
#4140=AXIS2_PLACEMENT_3D('',#6280,#5006,#5007);
#4141=AXIS2_PLACEMENT_3D('',#6286,#5011,#5012);
#4142=AXIS2_PLACEMENT_3D('',#6292,#5016,#5017);
#4143=AXIS2_PLACEMENT_3D('',#6298,#5021,#5022);
#4144=AXIS2_PLACEMENT_3D('',#6304,#5026,#5027);
#4145=AXIS2_PLACEMENT_3D('',#6310,#5031,#5032);
#4146=AXIS2_PLACEMENT_3D('',#6316,#5036,#5037);
#4147=AXIS2_PLACEMENT_3D('',#6322,#5041,#5042);
#4148=AXIS2_PLACEMENT_3D('',#6328,#5046,#5047);
#4149=AXIS2_PLACEMENT_3D('',#6334,#5051,#5052);
#4150=AXIS2_PLACEMENT_3D('',#6336,#5053,#5054);
#4151=AXIS2_PLACEMENT_3D('',#6338,#5056,#5057);
#4152=AXIS2_PLACEMENT_3D('',#6339,#5058,#5059);
#4153=AXIS2_PLACEMENT_3D('',#6340,#5060,#5061);
#4154=AXIS2_PLACEMENT_3D('',#6341,#5062,#5063);
#4155=AXIS2_PLACEMENT_3D('',#6343,#5064,#5065);
#4156=AXIS2_PLACEMENT_3D('',#6347,#5067,#5068);
#4157=AXIS2_PLACEMENT_3D('',#6350,#5070,#5071);
#4158=AXIS2_PLACEMENT_3D('',#6351,#5072,#5073);
#4159=AXIS2_PLACEMENT_3D('',#6352,#5074,#5075);
#4160=AXIS2_PLACEMENT_3D('',#6353,#5076,#5077);
#4161=AXIS2_PLACEMENT_3D('',#6354,#5078,#5079);
#4162=AXIS2_PLACEMENT_3D('',#6355,#5080,#5081);
#4163=AXIS2_PLACEMENT_3D('',#6356,#5082,#5083);
#4164=AXIS2_PLACEMENT_3D('',#6357,#5084,#5085);
#4165=AXIS2_PLACEMENT_3D('',#6358,#5086,#5087);
#4166=AXIS2_PLACEMENT_3D('',#6359,#5088,#5089);
#4167=AXIS2_PLACEMENT_3D('',#6360,#5090,#5091);
#4168=AXIS2_PLACEMENT_3D('',#6361,#5092,#5093);
#4169=AXIS2_PLACEMENT_3D('',#6362,#5094,#5095);
#4170=AXIS2_PLACEMENT_3D('',#6363,#5096,#5097);
#4171=AXIS2_PLACEMENT_3D('',#6364,#5098,#5099);
#4172=AXIS2_PLACEMENT_3D('',#6365,#5100,#5101);
#4173=AXIS2_PLACEMENT_3D('',#6367,#5102,#5103);
#4174=AXIS2_PLACEMENT_3D('',#6369,#5105,#5106);
#4175=AXIS2_PLACEMENT_3D('',#6370,#5107,#5108);
#4176=AXIS2_PLACEMENT_3D('',#6371,#5109,#5110);
#4177=AXIS2_PLACEMENT_3D('',#6372,#5111,#5112);
#4178=AXIS2_PLACEMENT_3D('',#6373,#5113,#5114);
#4179=AXIS2_PLACEMENT_3D('',#6374,#5115,#5116);
#4180=AXIS2_PLACEMENT_3D('',#6375,#5117,#5118);
#4181=AXIS2_PLACEMENT_3D('',#6376,#5119,#5120);
#4182=AXIS2_PLACEMENT_3D('',#6377,#5121,#5122);
#4183=AXIS2_PLACEMENT_3D('',#6378,#5123,#5124);
#4184=AXIS2_PLACEMENT_3D('',#6379,#5125,#5126);
#4185=AXIS2_PLACEMENT_3D('',#6382,#5128,#5129);
#4186=AXIS2_PLACEMENT_3D('',#6383,#5130,#5131);
#4187=AXIS2_PLACEMENT_3D('',#6384,#5132,#5133);
#4188=AXIS2_PLACEMENT_3D('',#6385,#5134,#5135);
#4189=AXIS2_PLACEMENT_3D('',#6386,#5136,#5137);
#4190=AXIS2_PLACEMENT_3D('',#6387,#5138,#5139);
#4191=AXIS2_PLACEMENT_3D('',#6388,#5140,#5141);
#4192=AXIS2_PLACEMENT_3D('',#6389,#5142,#5143);
#4193=AXIS2_PLACEMENT_3D('',#6390,#5144,#5145);
#4194=AXIS2_PLACEMENT_3D('',#6391,#5146,#5147);
#4195=AXIS2_PLACEMENT_3D('',#6392,#5148,#5149);
#4196=AXIS2_PLACEMENT_3D('',#6393,#5150,#5151);
#4197=AXIS2_PLACEMENT_3D('',#6394,#5152,#5153);
#4198=AXIS2_PLACEMENT_3D('',#6395,#5154,#5155);
#4199=AXIS2_PLACEMENT_3D('',#6396,#5156,#5157);
#4200=AXIS2_PLACEMENT_3D('',#6397,#5158,#5159);
#4201=AXIS2_PLACEMENT_3D('',#6398,#5160,#5161);
#4202=AXIS2_PLACEMENT_3D('',#6399,#5162,#5163);
#4203=AXIS2_PLACEMENT_3D('',#6400,#5164,#5165);
#4204=AXIS2_PLACEMENT_3D('',#6401,#5166,#5167);
#4205=AXIS2_PLACEMENT_3D('',#6402,#5168,#5169);
#4206=AXIS2_PLACEMENT_3D('',#6403,#5170,#5171);
#4207=AXIS2_PLACEMENT_3D('',#6404,#5172,#5173);
#4208=AXIS2_PLACEMENT_3D('',#6405,#5174,#5175);
#4209=AXIS2_PLACEMENT_3D('',#6406,#5176,#5177);
#4210=AXIS2_PLACEMENT_3D('',#6407,#5178,#5179);
#4211=AXIS2_PLACEMENT_3D('',#6411,#5182,#5183);
#4212=AXIS2_PLACEMENT_3D('',#6414,#5185,#5186);
#4213=AXIS2_PLACEMENT_3D('',#6415,#5187,#5188);
#4214=AXIS2_PLACEMENT_3D('',#6417,#5190,#5191);
#4215=AXIS2_PLACEMENT_3D('',#6419,#5192,#5193);
#4216=AXIS2_PLACEMENT_3D('',#6421,#5195,#5196);
#4217=AXIS2_PLACEMENT_3D('',#6422,#5197,#5198);
#4218=AXIS2_PLACEMENT_3D('',#6423,#5199,#5200);
#4219=AXIS2_PLACEMENT_3D('',#6424,#5201,#5202);
#4220=AXIS2_PLACEMENT_3D('',#6425,#5203,#5204);
#4221=AXIS2_PLACEMENT_3D('',#6434,#5209,#5210);
#4222=AXIS2_PLACEMENT_3D('',#6443,#5215,#5216);
#4223=AXIS2_PLACEMENT_3D('',#6444,#5217,#5218);
#4224=AXIS2_PLACEMENT_3D('',#6445,#5219,#5220);
#4225=AXIS2_PLACEMENT_3D('',#6447,#5221,#5222);
#4226=AXIS2_PLACEMENT_3D('',#6449,#5223,#5224);
#4227=AXIS2_PLACEMENT_3D('',#6450,#5225,#5226);
#4228=AXIS2_PLACEMENT_3D('',#6452,#5227,#5228);
#4229=AXIS2_PLACEMENT_3D('',#6454,#5230,#5231);
#4230=AXIS2_PLACEMENT_3D('',#6455,#5232,#5233);
#4231=AXIS2_PLACEMENT_3D('',#6457,#5234,#5235);
#4232=AXIS2_PLACEMENT_3D('',#6459,#5237,#5238);
#4233=AXIS2_PLACEMENT_3D('',#6460,#5239,#5240);
#4234=AXIS2_PLACEMENT_3D('',#6461,#5241,#5242);
#4235=AXIS2_PLACEMENT_3D('',#6462,#5243,#5244);
#4236=AXIS2_PLACEMENT_3D('',#6463,#5245,#5246);
#4237=AXIS2_PLACEMENT_3D('',#6464,#5247,#5248);
#4238=AXIS2_PLACEMENT_3D('',#6465,#5249,#5250);
#4239=AXIS2_PLACEMENT_3D('',#6466,#5251,#5252);
#4240=AXIS2_PLACEMENT_3D('',#6475,#5257,#5258);
#4241=AXIS2_PLACEMENT_3D('',#6484,#5263,#5264);
#4242=AXIS2_PLACEMENT_3D('',#6485,#5265,#5266);
#4243=AXIS2_PLACEMENT_3D('',#6486,#5267,#5268);
#4244=AXIS2_PLACEMENT_3D('',#6488,#5269,#5270);
#4245=AXIS2_PLACEMENT_3D('',#6490,#5271,#5272);
#4246=AXIS2_PLACEMENT_3D('',#6491,#5273,#5274);
#4247=AXIS2_PLACEMENT_3D('',#6493,#5275,#5276);
#4248=AXIS2_PLACEMENT_3D('',#6495,#5278,#5279);
#4249=AXIS2_PLACEMENT_3D('',#6496,#5280,#5281);
#4250=AXIS2_PLACEMENT_3D('',#6498,#5282,#5283);
#4251=AXIS2_PLACEMENT_3D('',#6500,#5285,#5286);
#4252=AXIS2_PLACEMENT_3D('',#6501,#5287,#5288);
#4253=AXIS2_PLACEMENT_3D('',#6502,#5289,#5290);
#4254=AXIS2_PLACEMENT_3D('',#6503,#5291,#5292);
#4255=AXIS2_PLACEMENT_3D('',#6504,#5293,#5294);
#4256=AXIS2_PLACEMENT_3D('',#6505,#5295,#5296);
#4257=AXIS2_PLACEMENT_3D('',#6506,#5297,#5298);
#4258=AXIS2_PLACEMENT_3D('',#6507,#5299,#5300);
#4259=AXIS2_PLACEMENT_3D('',#6516,#5305,#5306);
#4260=AXIS2_PLACEMENT_3D('',#6525,#5311,#5312);
#4261=AXIS2_PLACEMENT_3D('',#6526,#5313,#5314);
#4262=AXIS2_PLACEMENT_3D('',#6527,#5315,#5316);
#4263=AXIS2_PLACEMENT_3D('',#6529,#5317,#5318);
#4264=AXIS2_PLACEMENT_3D('',#6531,#5319,#5320);
#4265=AXIS2_PLACEMENT_3D('',#6532,#5321,#5322);
#4266=AXIS2_PLACEMENT_3D('',#6534,#5323,#5324);
#4267=AXIS2_PLACEMENT_3D('',#6536,#5326,#5327);
#4268=AXIS2_PLACEMENT_3D('',#6537,#5328,#5329);
#4269=AXIS2_PLACEMENT_3D('',#6539,#5330,#5331);
#4270=AXIS2_PLACEMENT_3D('',#6541,#5333,#5334);
#4271=AXIS2_PLACEMENT_3D('',#6542,#5335,#5336);
#4272=AXIS2_PLACEMENT_3D('',#6543,#5337,#5338);
#4273=AXIS2_PLACEMENT_3D('',#6544,#5339,#5340);
#4274=AXIS2_PLACEMENT_3D('',#6545,#5341,#5342);
#4275=AXIS2_PLACEMENT_3D('',#6546,#5343,#5344);
#4276=AXIS2_PLACEMENT_3D('',#6547,#5345,#5346);
#4277=AXIS2_PLACEMENT_3D('',#6548,#5347,#5348);
#4278=AXIS2_PLACEMENT_3D('',#6557,#5353,#5354);
#4279=AXIS2_PLACEMENT_3D('',#6566,#5359,#5360);
#4280=AXIS2_PLACEMENT_3D('',#6567,#5361,#5362);
#4281=AXIS2_PLACEMENT_3D('',#6568,#5363,#5364);
#4282=AXIS2_PLACEMENT_3D('',#6570,#5365,#5366);
#4283=AXIS2_PLACEMENT_3D('',#6572,#5367,#5368);
#4284=AXIS2_PLACEMENT_3D('',#6573,#5369,#5370);
#4285=AXIS2_PLACEMENT_3D('',#6575,#5371,#5372);
#4286=AXIS2_PLACEMENT_3D('',#6577,#5374,#5375);
#4287=AXIS2_PLACEMENT_3D('',#6578,#5376,#5377);
#4288=AXIS2_PLACEMENT_3D('',#6580,#5378,#5379);
#4289=AXIS2_PLACEMENT_3D('',#6582,#5381,#5382);
#4290=AXIS2_PLACEMENT_3D('',#6583,#5383,#5384);
#4291=AXIS2_PLACEMENT_3D('',#6584,#5385,#5386);
#4292=AXIS2_PLACEMENT_3D('',#6585,#5387,#5388);
#4293=AXIS2_PLACEMENT_3D('',#6586,#5389,#5390);
#4294=AXIS2_PLACEMENT_3D('',#6587,#5391,#5392);
#4295=AXIS2_PLACEMENT_3D('',#6588,#5393,#5394);
#4296=AXIS2_PLACEMENT_3D('',#6589,#5395,#5396);
#4297=AXIS2_PLACEMENT_3D('',#6598,#5401,#5402);
#4298=AXIS2_PLACEMENT_3D('',#6607,#5407,#5408);
#4299=AXIS2_PLACEMENT_3D('',#6608,#5409,#5410);
#4300=AXIS2_PLACEMENT_3D('',#6609,#5411,#5412);
#4301=AXIS2_PLACEMENT_3D('',#6611,#5413,#5414);
#4302=AXIS2_PLACEMENT_3D('',#6613,#5415,#5416);
#4303=AXIS2_PLACEMENT_3D('',#6614,#5417,#5418);
#4304=AXIS2_PLACEMENT_3D('',#6616,#5419,#5420);
#4305=AXIS2_PLACEMENT_3D('',#6618,#5422,#5423);
#4306=AXIS2_PLACEMENT_3D('',#6619,#5424,#5425);
#4307=AXIS2_PLACEMENT_3D('',#6621,#5426,#5427);
#4308=AXIS2_PLACEMENT_3D('',#6623,#5429,#5430);
#4309=AXIS2_PLACEMENT_3D('',#6624,#5431,#5432);
#4310=AXIS2_PLACEMENT_3D('',#6625,#5433,#5434);
#4311=AXIS2_PLACEMENT_3D('',#6626,#5435,#5436);
#4312=AXIS2_PLACEMENT_3D('',#6627,#5437,#5438);
#4313=AXIS2_PLACEMENT_3D('',#6628,#5439,#5440);
#4314=AXIS2_PLACEMENT_3D('',#6629,#5441,#5442);
#4315=AXIS2_PLACEMENT_3D('',#6630,#5443,#5444);
#4316=AXIS2_PLACEMENT_3D('',#6639,#5449,#5450);
#4317=AXIS2_PLACEMENT_3D('',#6648,#5455,#5456);
#4318=AXIS2_PLACEMENT_3D('',#6649,#5457,#5458);
#4319=AXIS2_PLACEMENT_3D('',#6650,#5459,#5460);
#4320=AXIS2_PLACEMENT_3D('',#6652,#5461,#5462);
#4321=AXIS2_PLACEMENT_3D('',#6654,#5463,#5464);
#4322=AXIS2_PLACEMENT_3D('',#6655,#5465,#5466);
#4323=AXIS2_PLACEMENT_3D('',#6657,#5467,#5468);
#4324=AXIS2_PLACEMENT_3D('',#6659,#5470,#5471);
#4325=AXIS2_PLACEMENT_3D('',#6660,#5472,#5473);
#4326=AXIS2_PLACEMENT_3D('',#6662,#5474,#5475);
#4327=AXIS2_PLACEMENT_3D('',#6664,#5477,#5478);
#4328=AXIS2_PLACEMENT_3D('',#6665,#5479,#5480);
#4329=AXIS2_PLACEMENT_3D('',#6666,#5481,#5482);
#4330=AXIS2_PLACEMENT_3D('',#6667,#5483,#5484);
#4331=AXIS2_PLACEMENT_3D('',#6668,#5485,#5486);
#4332=AXIS2_PLACEMENT_3D('',#6669,#5487,#5488);
#4333=AXIS2_PLACEMENT_3D('',#6670,#5489,#5490);
#4334=AXIS2_PLACEMENT_3D('',#6671,#5491,#5492);
#4335=AXIS2_PLACEMENT_3D('',#6680,#5497,#5498);
#4336=AXIS2_PLACEMENT_3D('',#6689,#5503,#5504);
#4337=AXIS2_PLACEMENT_3D('',#6690,#5505,#5506);
#4338=AXIS2_PLACEMENT_3D('',#6691,#5507,#5508);
#4339=AXIS2_PLACEMENT_3D('',#6693,#5509,#5510);
#4340=AXIS2_PLACEMENT_3D('',#6695,#5511,#5512);
#4341=AXIS2_PLACEMENT_3D('',#6696,#5513,#5514);
#4342=AXIS2_PLACEMENT_3D('',#6698,#5515,#5516);
#4343=AXIS2_PLACEMENT_3D('',#6700,#5518,#5519);
#4344=AXIS2_PLACEMENT_3D('',#6701,#5520,#5521);
#4345=AXIS2_PLACEMENT_3D('',#6703,#5522,#5523);
#4346=AXIS2_PLACEMENT_3D('',#6705,#5525,#5526);
#4347=AXIS2_PLACEMENT_3D('',#6706,#5527,#5528);
#4348=AXIS2_PLACEMENT_3D('',#6707,#5529,#5530);
#4349=AXIS2_PLACEMENT_3D('',#6708,#5531,#5532);
#4350=AXIS2_PLACEMENT_3D('',#6709,#5533,#5534);
#4351=AXIS2_PLACEMENT_3D('',#6710,#5535,#5536);
#4352=AXIS2_PLACEMENT_3D('',#6711,#5537,#5538);
#4353=AXIS2_PLACEMENT_3D('',#6712,#5539,#5540);
#4354=AXIS2_PLACEMENT_3D('',#6713,#5541,#5542);
#4355=AXIS2_PLACEMENT_3D('',#6714,#5543,#5544);
#4356=AXIS2_PLACEMENT_3D('',#6715,#5545,#5546);
#4357=AXIS2_PLACEMENT_3D('',#6716,#5547,#5548);
#4358=AXIS2_PLACEMENT_3D('',#6717,#5549,#5550);
#4359=AXIS2_PLACEMENT_3D('',#6718,#5551,#5552);
#4360=AXIS2_PLACEMENT_3D('',#6719,#5553,#5554);
#4361=AXIS2_PLACEMENT_3D('',#6720,#5555,#5556);
#4362=AXIS2_PLACEMENT_3D('',#6721,#5557,#5558);
#4363=AXIS2_PLACEMENT_3D('',#6722,#5559,#5560);
#4364=AXIS2_PLACEMENT_3D('',#6723,#5561,#5562);
#4365=DIRECTION('axis',(0.,0.,1.));
#4366=DIRECTION('refdir',(1.,0.,0.));
#4367=DIRECTION('axis',(0.,0.,1.));
#4368=DIRECTION('refdir',(1.,0.,0.));
#4369=DIRECTION('center_axis',(0.,1.,0.));
#4370=DIRECTION('ref_axis',(1.,0.,0.));
#4371=DIRECTION('',(0.,1.,0.));
#4372=DIRECTION('center_axis',(0.,1.,0.));
#4373=DIRECTION('ref_axis',(1.,0.,0.));
#4374=DIRECTION('',(0.,1.,0.));
#4375=DIRECTION('center_axis',(0.,1.,0.));
#4376=DIRECTION('ref_axis',(1.,0.,0.));
#4377=DIRECTION('center_axis',(0.,1.,0.));
#4378=DIRECTION('ref_axis',(1.,0.,0.));
#4379=DIRECTION('',(0.,1.,0.));
#4380=DIRECTION('center_axis',(0.,-1.,0.));
#4381=DIRECTION('ref_axis',(1.,0.,0.));
#4382=DIRECTION('center_axis',(0.,1.,0.));
#4383=DIRECTION('ref_axis',(1.,0.,0.));
#4384=DIRECTION('center_axis',(0.,-1.,0.));
#4385=DIRECTION('ref_axis',(1.,0.,0.));
#4386=DIRECTION('center_axis',(0.,1.,0.));
#4387=DIRECTION('ref_axis',(1.,0.,0.));
#4388=DIRECTION('',(-0.795671922146114,0.,0.605727820318918));
#4389=DIRECTION('center_axis',(0.,-1.,0.));
#4390=DIRECTION('ref_axis',(1.,0.,0.));
#4391=DIRECTION('center_axis',(0.,-1.,0.));
#4392=DIRECTION('ref_axis',(1.,0.,0.));
#4393=DIRECTION('',(-0.795671922146114,0.,-0.605727820318918));
#4394=DIRECTION('center_axis',(0.605727820318918,0.,-0.795671922146114));
#4395=DIRECTION('ref_axis',(-0.795671922146114,0.,-0.605727820318918));
#4396=DIRECTION('',(0.,-1.,0.));
#4397=DIRECTION('',(-0.795671922146114,0.,-0.605727820318918));
#4398=DIRECTION('center_axis',(-0.605727820318918,0.,-0.795671922146114));
#4399=DIRECTION('ref_axis',(-0.795671922146114,0.,0.605727820318918));
#4400=DIRECTION('',(-0.795671922146114,0.,0.605727820318918));
#4401=DIRECTION('',(0.,1.,0.));
#4402=DIRECTION('center_axis',(0.,1.,0.));
#4403=DIRECTION('ref_axis',(1.,0.,0.));
#4404=DIRECTION('center_axis',(0.,1.,0.));
#4405=DIRECTION('ref_axis',(1.,0.,0.));
#4406=DIRECTION('center_axis',(0.,1.,0.));
#4407=DIRECTION('ref_axis',(1.,0.,0.));
#4408=DIRECTION('center_axis',(0.,-1.,0.));
#4409=DIRECTION('ref_axis',(1.,0.,0.));
#4410=DIRECTION('',(0.,-1.,0.));
#4411=DIRECTION('center_axis',(0.,1.,0.));
#4412=DIRECTION('ref_axis',(1.,0.,0.));
#4413=DIRECTION('center_axis',(0.,1.,0.));
#4414=DIRECTION('ref_axis',(1.,0.,0.));
#4415=DIRECTION('',(0.,-1.,0.));
#4416=DIRECTION('center_axis',(0.,1.,0.));
#4417=DIRECTION('ref_axis',(1.,0.,0.));
#4418=DIRECTION('axis',(0.,0.,1.));
#4419=DIRECTION('refdir',(1.,0.,0.));
#4420=DIRECTION('center_axis',(6.12323399573676E-17,0.,1.));
#4421=DIRECTION('ref_axis',(1.,0.,0.));
#4422=DIRECTION('center_axis',(0.,0.,1.));
#4423=DIRECTION('ref_axis',(1.,0.,0.));
#4424=DIRECTION('center_axis',(1.11022302462516E-16,-1.,0.));
#4425=DIRECTION('ref_axis',(-1.,-1.11022302462516E-16,0.));
#4426=DIRECTION('center_axis',(0.,0.,1.));
#4427=DIRECTION('ref_axis',(1.,0.,0.));
#4428=DIRECTION('',(0.,0.,-1.));
#4429=DIRECTION('center_axis',(0.,0.,1.));
#4430=DIRECTION('ref_axis',(1.,0.,0.));
#4431=DIRECTION('center_axis',(0.,0.,1.));
#4432=DIRECTION('ref_axis',(1.,0.,0.));
#4433=DIRECTION('center_axis',(0.,0.,1.));
#4434=DIRECTION('ref_axis',(1.,0.,0.));
#4435=DIRECTION('center_axis',(0.,0.,-1.));
#4436=DIRECTION('ref_axis',(1.,0.,0.));
#4437=DIRECTION('center_axis',(0.,0.,-1.));
#4438=DIRECTION('ref_axis',(1.,0.,0.));
#4439=DIRECTION('',(0.,0.,1.));
#4440=DIRECTION('center_axis',(0.,0.,1.));
#4441=DIRECTION('ref_axis',(1.,0.,0.));
#4442=DIRECTION('axis',(0.,0.,1.));
#4443=DIRECTION('refdir',(1.,0.,0.));
#4444=DIRECTION('center_axis',(-0.707106781186547,0.,0.707106781186548));
#4445=DIRECTION('ref_axis',(0.707106781186548,0.,0.707106781186547));
#4446=DIRECTION('',(0.707106781186548,0.,0.707106781186547));
#4447=DIRECTION('',(0.,-1.,0.));
#4448=DIRECTION('',(-0.707106781186548,0.,-0.707106781186547));
#4449=DIRECTION('',(0.,1.,0.));
#4450=DIRECTION('center_axis',(1.,0.,0.));
#4451=DIRECTION('ref_axis',(0.,0.,-1.));
#4452=DIRECTION('',(0.,0.,-1.));
#4453=DIRECTION('',(0.,-1.,0.));
#4454=DIRECTION('',(0.,0.,1.));
#4455=DIRECTION('',(0.,1.,0.));
#4456=DIRECTION('center_axis',(0.,1.,0.));
#4457=DIRECTION('ref_axis',(1.,0.,0.));
#4458=DIRECTION('center_axis',(0.,1.,0.));
#4459=DIRECTION('ref_axis',(1.,0.,0.));
#4460=DIRECTION('center_axis',(0.,-1.,0.));
#4461=DIRECTION('ref_axis',(1.,0.,0.));
#4462=DIRECTION('center_axis',(0.,1.,0.));
#4463=DIRECTION('ref_axis',(1.,0.,0.));
#4464=DIRECTION('center_axis',(0.,1.,0.));
#4465=DIRECTION('ref_axis',(1.,0.,0.));
#4466=DIRECTION('center_axis',(0.,-1.,0.));
#4467=DIRECTION('ref_axis',(1.,0.,0.));
#4468=DIRECTION('center_axis',(0.,-1.,0.));
#4469=DIRECTION('ref_axis',(1.,0.,0.));
#4470=DIRECTION('',(0.,1.,0.));
#4471=DIRECTION('center_axis',(0.,1.,0.));
#4472=DIRECTION('ref_axis',(1.,0.,0.));
#4473=DIRECTION('center_axis',(0.,-1.,0.));
#4474=DIRECTION('ref_axis',(1.,0.,0.));
#4475=DIRECTION('center_axis',(0.,-1.,0.));
#4476=DIRECTION('ref_axis',(1.,0.,0.));
#4477=DIRECTION('',(0.,1.,0.));
#4478=DIRECTION('center_axis',(0.,1.,0.));
#4479=DIRECTION('ref_axis',(1.,0.,0.));
#4480=DIRECTION('center_axis',(0.,1.,0.));
#4481=DIRECTION('ref_axis',(1.,0.,0.));
#4482=DIRECTION('center_axis',(0.,-1.,0.));
#4483=DIRECTION('ref_axis',(1.,0.,0.));
#4484=DIRECTION('center_axis',(0.,1.,0.));
#4485=DIRECTION('ref_axis',(1.,0.,0.));
#4486=DIRECTION('center_axis',(0.,1.,0.));
#4487=DIRECTION('ref_axis',(1.,0.,0.));
#4488=DIRECTION('center_axis',(0.,1.,0.));
#4489=DIRECTION('ref_axis',(1.,0.,0.));
#4490=DIRECTION('axis',(0.,0.,1.));
#4491=DIRECTION('refdir',(1.,0.,0.));
#4492=DIRECTION('center_axis',(0.,1.,0.));
#4493=DIRECTION('ref_axis',(-1.,0.,0.));
#4494=DIRECTION('center_axis',(0.,-1.,0.));
#4495=DIRECTION('ref_axis',(1.,0.,0.));
#4496=DIRECTION('',(0.,0.,1.));
#4497=DIRECTION('center_axis',(0.,1.,0.));
#4498=DIRECTION('ref_axis',(1.,0.,0.));
#4499=DIRECTION('',(0.,0.,1.));
#4500=DIRECTION('center_axis',(-1.,0.,0.));
#4501=DIRECTION('ref_axis',(0.,-1.,0.));
#4502=DIRECTION('',(0.,-1.,0.));
#4503=DIRECTION('',(0.,1.,0.));
#4504=DIRECTION('',(0.,0.,1.));
#4505=DIRECTION('center_axis',(1.,0.,0.));
#4506=DIRECTION('ref_axis',(0.,1.,0.));
#4507=DIRECTION('',(0.,1.,0.));
#4508=DIRECTION('',(0.,0.,1.));
#4509=DIRECTION('',(0.,-1.,0.));
#4510=DIRECTION('center_axis',(0.,1.,0.));
#4511=DIRECTION('ref_axis',(1.,0.,0.));
#4512=DIRECTION('center_axis',(0.,-1.,0.));
#4513=DIRECTION('ref_axis',(1.,0.,0.));
#4514=DIRECTION('',(0.,-1.,0.));
#4515=DIRECTION('center_axis',(0.,1.,0.));
#4516=DIRECTION('ref_axis',(1.,0.,0.));
#4517=DIRECTION('center_axis',(0.,1.,0.));
#4518=DIRECTION('ref_axis',(1.,0.,0.));
#4519=DIRECTION('center_axis',(0.,1.,0.));
#4520=DIRECTION('ref_axis',(1.,0.,0.));
#4521=DIRECTION('center_axis',(0.,1.,0.));
#4522=DIRECTION('ref_axis',(1.,0.,0.));
#4523=DIRECTION('',(0.,-1.,0.));
#4524=DIRECTION('center_axis',(0.,-1.,0.));
#4525=DIRECTION('ref_axis',(1.,0.,0.));
#4526=DIRECTION('center_axis',(0.,-1.,0.));
#4527=DIRECTION('ref_axis',(1.,0.,0.));
#4528=DIRECTION('center_axis',(0.,-1.,0.));
#4529=DIRECTION('ref_axis',(1.,0.,0.));
#4530=DIRECTION('center_axis',(0.,1.,0.));
#4531=DIRECTION('ref_axis',(1.,0.,0.));
#4532=DIRECTION('center_axis',(0.,-1.,0.));
#4533=DIRECTION('ref_axis',(1.,0.,0.));
#4534=DIRECTION('',(0.,-1.,0.));
#4535=DIRECTION('center_axis',(0.,1.,0.));
#4536=DIRECTION('ref_axis',(1.,0.,0.));
#4537=DIRECTION('center_axis',(0.,1.,0.));
#4538=DIRECTION('ref_axis',(1.,0.,0.));
#4539=DIRECTION('center_axis',(0.,-1.,0.));
#4540=DIRECTION('ref_axis',(1.,0.,0.));
#4541=DIRECTION('',(0.,-1.,0.));
#4542=DIRECTION('center_axis',(0.,1.,0.));
#4543=DIRECTION('ref_axis',(1.,0.,0.));
#4544=DIRECTION('center_axis',(0.,1.,0.));
#4545=DIRECTION('ref_axis',(1.,0.,0.));
#4546=DIRECTION('center_axis',(0.,-1.,0.));
#4547=DIRECTION('ref_axis',(1.,0.,0.));
#4548=DIRECTION('',(0.,-1.,0.));
#4549=DIRECTION('center_axis',(0.,1.,0.));
#4550=DIRECTION('ref_axis',(1.,0.,0.));
#4551=DIRECTION('center_axis',(0.,1.,0.));
#4552=DIRECTION('ref_axis',(1.,0.,0.));
#4553=DIRECTION('center_axis',(0.,-1.,0.));
#4554=DIRECTION('ref_axis',(1.,0.,0.));
#4555=DIRECTION('',(0.,-1.,0.));
#4556=DIRECTION('center_axis',(0.,1.,0.));
#4557=DIRECTION('ref_axis',(1.,0.,0.));
#4558=DIRECTION('center_axis',(0.,1.,0.));
#4559=DIRECTION('ref_axis',(1.,0.,0.));
#4560=DIRECTION('center_axis',(0.,-1.,0.));
#4561=DIRECTION('ref_axis',(1.,0.,0.));
#4562=DIRECTION('',(0.,-1.,0.));
#4563=DIRECTION('center_axis',(0.,1.,0.));
#4564=DIRECTION('ref_axis',(1.,0.,0.));
#4565=DIRECTION('center_axis',(0.,1.,0.));
#4566=DIRECTION('ref_axis',(1.,0.,0.));
#4567=DIRECTION('center_axis',(0.,-1.,0.));
#4568=DIRECTION('ref_axis',(1.,0.,0.));
#4569=DIRECTION('',(0.,-1.,0.));
#4570=DIRECTION('center_axis',(0.,1.,0.));
#4571=DIRECTION('ref_axis',(1.,0.,0.));
#4572=DIRECTION('center_axis',(0.,1.,0.));
#4573=DIRECTION('ref_axis',(1.,0.,0.));
#4574=DIRECTION('center_axis',(0.,-1.,0.));
#4575=DIRECTION('ref_axis',(1.,0.,0.));
#4576=DIRECTION('',(0.,-1.,0.));
#4577=DIRECTION('center_axis',(0.,1.,0.));
#4578=DIRECTION('ref_axis',(1.,0.,0.));
#4579=DIRECTION('center_axis',(0.,1.,0.));
#4580=DIRECTION('ref_axis',(1.,0.,0.));
#4581=DIRECTION('center_axis',(0.,-1.,0.));
#4582=DIRECTION('ref_axis',(1.,0.,0.));
#4583=DIRECTION('',(0.,-1.,0.));
#4584=DIRECTION('center_axis',(0.,1.,0.));
#4585=DIRECTION('ref_axis',(1.,0.,0.));
#4586=DIRECTION('center_axis',(0.,1.,0.));
#4587=DIRECTION('ref_axis',(1.,0.,0.));
#4588=DIRECTION('center_axis',(0.,-1.,0.));
#4589=DIRECTION('ref_axis',(1.,0.,0.));
#4590=DIRECTION('',(0.,-1.,0.));
#4591=DIRECTION('center_axis',(0.,1.,0.));
#4592=DIRECTION('ref_axis',(1.,0.,0.));
#4593=DIRECTION('center_axis',(0.,1.,0.));
#4594=DIRECTION('ref_axis',(1.,0.,0.));
#4595=DIRECTION('center_axis',(0.,-1.,0.));
#4596=DIRECTION('ref_axis',(1.,0.,0.));
#4597=DIRECTION('',(0.,-1.,0.));
#4598=DIRECTION('center_axis',(0.,1.,0.));
#4599=DIRECTION('ref_axis',(1.,0.,0.));
#4600=DIRECTION('center_axis',(0.,1.,0.));
#4601=DIRECTION('ref_axis',(1.,0.,0.));
#4602=DIRECTION('center_axis',(0.,-1.,0.));
#4603=DIRECTION('ref_axis',(1.,0.,0.));
#4604=DIRECTION('',(0.,-1.,0.));
#4605=DIRECTION('center_axis',(0.,1.,0.));
#4606=DIRECTION('ref_axis',(1.,0.,0.));
#4607=DIRECTION('center_axis',(0.,1.,0.));
#4608=DIRECTION('ref_axis',(1.,0.,0.));
#4609=DIRECTION('center_axis',(0.,-1.,0.));
#4610=DIRECTION('ref_axis',(1.,0.,0.));
#4611=DIRECTION('',(0.,-1.,0.));
#4612=DIRECTION('center_axis',(0.,1.,0.));
#4613=DIRECTION('ref_axis',(1.,0.,0.));
#4614=DIRECTION('center_axis',(0.,1.,0.));
#4615=DIRECTION('ref_axis',(1.,0.,0.));
#4616=DIRECTION('center_axis',(0.,-1.,0.));
#4617=DIRECTION('ref_axis',(1.,0.,0.));
#4618=DIRECTION('',(0.,-1.,0.));
#4619=DIRECTION('center_axis',(0.,1.,0.));
#4620=DIRECTION('ref_axis',(1.,0.,0.));
#4621=DIRECTION('center_axis',(0.,1.,0.));
#4622=DIRECTION('ref_axis',(1.,0.,0.));
#4623=DIRECTION('center_axis',(0.,-1.,0.));
#4624=DIRECTION('ref_axis',(1.,0.,0.));
#4625=DIRECTION('',(0.,-1.,0.));
#4626=DIRECTION('center_axis',(0.,1.,0.));
#4627=DIRECTION('ref_axis',(1.,0.,0.));
#4628=DIRECTION('center_axis',(0.,1.,0.));
#4629=DIRECTION('ref_axis',(1.,0.,0.));
#4630=DIRECTION('center_axis',(0.,-1.,0.));
#4631=DIRECTION('ref_axis',(1.,0.,0.));
#4632=DIRECTION('',(0.,-1.,0.));
#4633=DIRECTION('center_axis',(0.,1.,0.));
#4634=DIRECTION('ref_axis',(1.,0.,0.));
#4635=DIRECTION('center_axis',(0.,1.,0.));
#4636=DIRECTION('ref_axis',(1.,0.,0.));
#4637=DIRECTION('center_axis',(0.,-1.,0.));
#4638=DIRECTION('ref_axis',(1.,0.,0.));
#4639=DIRECTION('',(0.,-1.,0.));
#4640=DIRECTION('center_axis',(0.,1.,0.));
#4641=DIRECTION('ref_axis',(1.,0.,0.));
#4642=DIRECTION('center_axis',(0.,1.,0.));
#4643=DIRECTION('ref_axis',(1.,0.,0.));
#4644=DIRECTION('center_axis',(0.,-1.,0.));
#4645=DIRECTION('ref_axis',(1.,0.,0.));
#4646=DIRECTION('',(0.,-1.,0.));
#4647=DIRECTION('center_axis',(0.,1.,0.));
#4648=DIRECTION('ref_axis',(1.,0.,0.));
#4649=DIRECTION('center_axis',(0.,-1.,0.));
#4650=DIRECTION('ref_axis',(1.,0.,0.));
#4651=DIRECTION('center_axis',(0.,-1.,0.));
#4652=DIRECTION('ref_axis',(1.,0.,0.));
#4653=DIRECTION('axis',(0.,0.,1.));
#4654=DIRECTION('refdir',(1.,0.,0.));
#4655=DIRECTION('center_axis',(0.,1.,0.));
#4656=DIRECTION('ref_axis',(1.,0.,0.));
#4657=DIRECTION('center_axis',(0.,-1.,0.));
#4658=DIRECTION('ref_axis',(1.,0.,0.));
#4659=DIRECTION('center_axis',(0.,1.,0.));
#4660=DIRECTION('ref_axis',(0.,0.,1.));
#4661=DIRECTION('center_axis',(0.,1.,0.));
#4662=DIRECTION('ref_axis',(1.,0.,0.));
#4663=DIRECTION('center_axis',(0.,1.,0.));
#4664=DIRECTION('ref_axis',(1.,0.,0.));
#4665=DIRECTION('center_axis',(0.,1.,0.));
#4666=DIRECTION('ref_axis',(1.,0.,0.));
#4667=DIRECTION('center_axis',(0.,-1.,0.));
#4668=DIRECTION('ref_axis',(0.,0.,-1.));
#4669=DIRECTION('center_axis',(6.12323399573677E-17,0.,1.));
#4670=DIRECTION('ref_axis',(1.,0.,0.));
#4671=DIRECTION('center_axis',(0.,0.,-1.));
#4672=DIRECTION('ref_axis',(1.,0.,0.));
#4673=DIRECTION('center_axis',(6.12323399573677E-17,0.,1.));
#4674=DIRECTION('ref_axis',(1.,0.,0.));
#4675=DIRECTION('center_axis',(0.,0.,-1.));
#4676=DIRECTION('ref_axis',(1.,0.,0.));
#4677=DIRECTION('center_axis',(0.,0.,1.));
#4678=DIRECTION('ref_axis',(1.,0.,0.));
#4679=DIRECTION('center_axis',(0.,0.,1.));
#4680=DIRECTION('ref_axis',(1.,0.,0.));
#4681=DIRECTION('',(-0.707106781186547,8.65956056235493E-17,0.707106781186548));
#4682=DIRECTION('center_axis',(0.,0.,-1.));
#4683=DIRECTION('ref_axis',(1.,0.,0.));
#4684=DIRECTION('center_axis',(0.,0.,-1.));
#4685=DIRECTION('ref_axis',(1.,0.,0.));
#4686=DIRECTION('center_axis',(0.,0.,-1.));
#4687=DIRECTION('ref_axis',(-1.,0.,0.));
#4688=DIRECTION('',(0.,0.,1.));
#4689=DIRECTION('center_axis',(0.,0.,-1.));
#4690=DIRECTION('ref_axis',(1.,0.,0.));
#4691=DIRECTION('center_axis',(0.,0.,-1.));
#4692=DIRECTION('ref_axis',(-1.,0.,0.));
#4693=DIRECTION('center_axis',(0.,0.,-1.));
#4694=DIRECTION('ref_axis',(-1.,0.,0.));
#4695=DIRECTION('',(-0.311881116775508,3.81944211373628E-17,0.9501211338555));
#4696=DIRECTION('axis',(0.,0.,1.));
#4697=DIRECTION('refdir',(1.,0.,0.));
#4698=DIRECTION('center_axis',(0.,0.,-1.));
#4699=DIRECTION('ref_axis',(1.,0.,0.));
#4700=DIRECTION('',(0.,0.,-1.));
#4701=DIRECTION('center_axis',(0.,0.,-1.));
#4702=DIRECTION('ref_axis',(1.,0.,0.));
#4703=DIRECTION('center_axis',(0.,0.,1.));
#4704=DIRECTION('ref_axis',(1.,0.,0.));
#4705=DIRECTION('center_axis',(-0.951056516295154,0.,0.309016994374948));
#4706=DIRECTION('ref_axis',(-0.309016994374948,0.,-0.951056516295154));
#4707=DIRECTION('',(0.,-1.,0.));
#4708=DIRECTION('',(-0.309016994374948,0.,-0.951056516295154));
#4709=DIRECTION('',(0.,1.,0.));
#4710=DIRECTION('',(0.309016994374948,0.,0.951056516295154));
#4711=DIRECTION('center_axis',(-0.309016994374948,0.,-0.951056516295154));
#4712=DIRECTION('ref_axis',(0.951056516295154,0.,-0.309016994374948));
#4713=DIRECTION('',(0.,-1.,0.));
#4714=DIRECTION('',(0.951056516295154,0.,-0.309016994374948));
#4715=DIRECTION('',(0.,1.,0.));
#4716=DIRECTION('',(-0.951056516295154,0.,0.309016994374948));
#4717=DIRECTION('center_axis',(-0.587785252292473,0.,-0.809016994374947));
#4718=DIRECTION('ref_axis',(0.809016994374947,0.,-0.587785252292473));
#4719=DIRECTION('',(0.,-1.,0.));
#4720=DIRECTION('',(0.809016994374947,0.,-0.587785252292473));
#4721=DIRECTION('',(0.,1.,0.));
#4722=DIRECTION('',(-0.809016994374947,0.,0.587785252292473));
#4723=DIRECTION('center_axis',(-0.809016994374948,0.,-0.587785252292473));
#4724=DIRECTION('ref_axis',(0.587785252292473,0.,-0.809016994374947));
#4725=DIRECTION('',(0.,-1.,0.));
#4726=DIRECTION('',(0.587785252292473,0.,-0.809016994374947));
#4727=DIRECTION('',(0.,1.,0.));
#4728=DIRECTION('',(-0.587785252292473,0.,0.809016994374947));
#4729=DIRECTION('center_axis',(-0.951056516295154,0.,-0.309016994374947));
#4730=DIRECTION('ref_axis',(0.309016994374947,0.,-0.951056516295154));
#4731=DIRECTION('',(0.,-1.,0.));
#4732=DIRECTION('',(0.309016994374947,0.,-0.951056516295154));
#4733=DIRECTION('',(0.,1.,0.));
#4734=DIRECTION('',(-0.309016994374947,0.,0.951056516295154));
#4735=DIRECTION('center_axis',(-1.,0.,1.11022302462516E-16));
#4736=DIRECTION('ref_axis',(-1.11022302462516E-16,0.,-1.));
#4737=DIRECTION('',(0.,-1.,0.));
#4738=DIRECTION('',(-1.11022302462516E-16,0.,-1.));
#4739=DIRECTION('',(0.,1.,0.));
#4740=DIRECTION('',(1.11022302462516E-16,0.,1.));
#4741=DIRECTION('center_axis',(-0.809016994374947,0.,0.587785252292473));
#4742=DIRECTION('ref_axis',(-0.587785252292473,0.,-0.809016994374947));
#4743=DIRECTION('',(0.,-1.,0.));
#4744=DIRECTION('',(-0.587785252292473,0.,-0.809016994374947));
#4745=DIRECTION('',(0.,1.,0.));
#4746=DIRECTION('',(0.587785252292473,0.,0.809016994374947));
#4747=DIRECTION('center_axis',(-0.587785252292473,0.,0.809016994374947));
#4748=DIRECTION('ref_axis',(-0.809016994374947,0.,-0.587785252292473));
#4749=DIRECTION('',(0.,-1.,0.));
#4750=DIRECTION('',(-0.809016994374947,0.,-0.587785252292473));
#4751=DIRECTION('',(0.,1.,0.));
#4752=DIRECTION('',(0.809016994374947,0.,0.587785252292473));
#4753=DIRECTION('center_axis',(-0.309016994374947,0.,0.951056516295154));
#4754=DIRECTION('ref_axis',(-0.951056516295154,0.,-0.309016994374947));
#4755=DIRECTION('',(0.,-1.,0.));
#4756=DIRECTION('',(-0.951056516295154,0.,-0.309016994374947));
#4757=DIRECTION('',(0.,1.,0.));
#4758=DIRECTION('',(0.951056516295154,0.,0.309016994374947));
#4759=DIRECTION('center_axis',(5.55111512312578E-17,0.,1.));
#4760=DIRECTION('ref_axis',(-1.,0.,5.55111512312578E-17));
#4761=DIRECTION('',(0.,-1.,0.));
#4762=DIRECTION('',(-1.,0.,5.55111512312578E-17));
#4763=DIRECTION('',(0.,1.,0.));
#4764=DIRECTION('',(1.,0.,-5.55111512312578E-17));
#4765=DIRECTION('center_axis',(0.309016994374948,0.,0.951056516295154));
#4766=DIRECTION('ref_axis',(-0.951056516295154,0.,0.309016994374948));
#4767=DIRECTION('',(0.,-1.,0.));
#4768=DIRECTION('',(-0.951056516295154,0.,0.309016994374948));
#4769=DIRECTION('',(0.,1.,0.));
#4770=DIRECTION('',(0.951056516295154,0.,-0.309016994374948));
#4771=DIRECTION('center_axis',(0.587785252292473,0.,0.809016994374947));
#4772=DIRECTION('ref_axis',(-0.809016994374947,0.,0.587785252292473));
#4773=DIRECTION('',(0.,-1.,0.));
#4774=DIRECTION('',(-0.809016994374947,0.,0.587785252292473));
#4775=DIRECTION('',(0.,1.,0.));
#4776=DIRECTION('',(0.809016994374947,0.,-0.587785252292473));
#4777=DIRECTION('center_axis',(0.809016994374948,0.,0.587785252292473));
#4778=DIRECTION('ref_axis',(-0.587785252292473,0.,0.809016994374947));
#4779=DIRECTION('',(0.,-1.,0.));
#4780=DIRECTION('',(-0.587785252292473,0.,0.809016994374947));
#4781=DIRECTION('',(0.,1.,0.));
#4782=DIRECTION('',(0.587785252292473,0.,-0.809016994374947));
#4783=DIRECTION('center_axis',(0.951056516295154,0.,0.309016994374947));
#4784=DIRECTION('ref_axis',(-0.309016994374947,0.,0.951056516295154));
#4785=DIRECTION('',(0.,-1.,0.));
#4786=DIRECTION('',(-0.309016994374947,0.,0.951056516295154));
#4787=DIRECTION('',(0.,1.,0.));
#4788=DIRECTION('',(0.309016994374947,0.,-0.951056516295154));
#4789=DIRECTION('center_axis',(0.951056516295154,0.,-0.309016994374948));
#4790=DIRECTION('ref_axis',(0.309016994374948,0.,0.951056516295154));
#4791=DIRECTION('',(0.,-1.,0.));
#4792=DIRECTION('',(0.309016994374948,0.,0.951056516295154));
#4793=DIRECTION('',(0.,1.,0.));
#4794=DIRECTION('',(-0.309016994374948,0.,-0.951056516295154));
#4795=DIRECTION('center_axis',(0.809016994374947,0.,-0.587785252292473));
#4796=DIRECTION('ref_axis',(0.587785252292473,0.,0.809016994374947));
#4797=DIRECTION('',(0.,-1.,0.));
#4798=DIRECTION('',(0.587785252292473,0.,0.809016994374947));
#4799=DIRECTION('',(0.,1.,0.));
#4800=DIRECTION('',(-0.587785252292473,0.,-0.809016994374947));
#4801=DIRECTION('center_axis',(0.587785252292473,0.,-0.809016994374947));
#4802=DIRECTION('ref_axis',(0.809016994374947,0.,0.587785252292473));
#4803=DIRECTION('',(0.,-1.,0.));
#4804=DIRECTION('',(0.809016994374947,0.,0.587785252292473));
#4805=DIRECTION('',(0.,1.,0.));
#4806=DIRECTION('',(-0.809016994374947,0.,-0.587785252292473));
#4807=DIRECTION('center_axis',(0.309016994374947,0.,-0.951056516295154));
#4808=DIRECTION('ref_axis',(0.951056516295154,0.,0.309016994374947));
#4809=DIRECTION('',(0.,-1.,0.));
#4810=DIRECTION('',(0.951056516295154,0.,0.309016994374947));
#4811=DIRECTION('',(0.,1.,0.));
#4812=DIRECTION('',(-0.951056516295154,0.,-0.309016994374947));
#4813=DIRECTION('center_axis',(-1.11022302462516E-16,0.,-1.));
#4814=DIRECTION('ref_axis',(1.,0.,-1.11022302462516E-16));
#4815=DIRECTION('',(0.,-1.,0.));
#4816=DIRECTION('',(1.,0.,-1.11022302462516E-16));
#4817=DIRECTION('',(0.,1.,0.));
#4818=DIRECTION('',(-1.,0.,1.11022302462516E-16));
#4819=DIRECTION('center_axis',(0.,-1.,0.));
#4820=DIRECTION('ref_axis',(0.309016994374947,0.,-0.951056516295154));
#4821=DIRECTION('center_axis',(0.,-1.,0.));
#4822=DIRECTION('ref_axis',(1.,0.,0.));
#4823=DIRECTION('',(-1.,0.,2.77555756156289E-16));
#4824=DIRECTION('center_axis',(0.,1.,0.));
#4825=DIRECTION('ref_axis',(1.,0.,0.));
#4826=DIRECTION('center_axis',(0.,1.,0.));
#4827=DIRECTION('ref_axis',(1.,0.,0.));
#4828=DIRECTION('center_axis',(0.,-1.,0.));
#4829=DIRECTION('ref_axis',(1.,0.,0.));
#4830=DIRECTION('center_axis',(0.,-1.,0.));
#4831=DIRECTION('ref_axis',(0.309016994374947,0.,-0.951056516295154));
#4832=DIRECTION('center_axis',(0.,-1.,0.));
#4833=DIRECTION('ref_axis',(1.,0.,0.));
#4834=DIRECTION('',(-0.951056516295154,0.,-0.309016994374947));
#4835=DIRECTION('center_axis',(0.,1.,0.));
#4836=DIRECTION('ref_axis',(1.,0.,0.));
#4837=DIRECTION('center_axis',(0.,-1.,0.));
#4838=DIRECTION('ref_axis',(0.309016994374947,0.,-0.951056516295154));
#4839=DIRECTION('center_axis',(0.,-1.,0.));
#4840=DIRECTION('ref_axis',(1.,0.,0.));
#4841=DIRECTION('',(-0.809016994374948,0.,-0.587785252292473));
#4842=DIRECTION('center_axis',(0.,1.,0.));
#4843=DIRECTION('ref_axis',(1.,0.,0.));
#4844=DIRECTION('center_axis',(0.,-1.,0.));
#4845=DIRECTION('ref_axis',(0.309016994374947,0.,-0.951056516295154));
#4846=DIRECTION('center_axis',(0.,-1.,0.));
#4847=DIRECTION('ref_axis',(1.,0.,0.));
#4848=DIRECTION('',(-0.587785252292473,0.,-0.809016994374947));
#4849=DIRECTION('center_axis',(0.,1.,0.));
#4850=DIRECTION('ref_axis',(1.,0.,0.));
#4851=DIRECTION('center_axis',(0.,-1.,0.));
#4852=DIRECTION('ref_axis',(0.309016994374947,0.,-0.951056516295154));
#4853=DIRECTION('center_axis',(0.,-1.,0.));
#4854=DIRECTION('ref_axis',(1.,0.,0.));
#4855=DIRECTION('',(-0.309016994374948,0.,-0.951056516295153));
#4856=DIRECTION('center_axis',(0.,1.,0.));
#4857=DIRECTION('ref_axis',(1.,0.,0.));
#4858=DIRECTION('center_axis',(0.,-1.,0.));
#4859=DIRECTION('ref_axis',(0.309016994374947,0.,-0.951056516295154));
#4860=DIRECTION('center_axis',(0.,-1.,0.));
#4861=DIRECTION('ref_axis',(1.,0.,0.));
#4862=DIRECTION('',(0.309016994374947,0.,-0.951056516295154));
#4863=DIRECTION('center_axis',(0.,1.,0.));
#4864=DIRECTION('ref_axis',(1.,0.,0.));
#4865=DIRECTION('center_axis',(0.,-1.,0.));
#4866=DIRECTION('ref_axis',(0.309016994374947,0.,-0.951056516295154));
#4867=DIRECTION('center_axis',(0.,-1.,0.));
#4868=DIRECTION('ref_axis',(1.,0.,0.));
#4869=DIRECTION('',(0.587785252292473,0.,-0.809016994374947));
#4870=DIRECTION('center_axis',(0.,1.,0.));
#4871=DIRECTION('ref_axis',(1.,0.,0.));
#4872=DIRECTION('center_axis',(0.,-1.,0.));
#4873=DIRECTION('ref_axis',(0.309016994374947,0.,-0.951056516295154));
#4874=DIRECTION('center_axis',(0.,-1.,0.));
#4875=DIRECTION('ref_axis',(1.,0.,0.));
#4876=DIRECTION('',(0.809016994374947,0.,-0.587785252292473));
#4877=DIRECTION('center_axis',(0.,1.,0.));
#4878=DIRECTION('ref_axis',(1.,0.,0.));
#4879=DIRECTION('center_axis',(0.,-1.,0.));
#4880=DIRECTION('ref_axis',(0.309016994374947,0.,-0.951056516295154));
#4881=DIRECTION('center_axis',(0.,-1.,0.));
#4882=DIRECTION('ref_axis',(1.,0.,0.));
#4883=DIRECTION('',(0.951056516295154,0.,-0.309016994374948));
#4884=DIRECTION('center_axis',(0.,1.,0.));
#4885=DIRECTION('ref_axis',(1.,0.,0.));
#4886=DIRECTION('center_axis',(0.,-1.,0.));
#4887=DIRECTION('ref_axis',(0.309016994374947,0.,-0.951056516295154));
#4888=DIRECTION('center_axis',(0.,-1.,0.));
#4889=DIRECTION('ref_axis',(1.,0.,0.));
#4890=DIRECTION('',(1.,0.,-1.11022302462516E-16));
#4891=DIRECTION('center_axis',(0.,1.,0.));
#4892=DIRECTION('ref_axis',(1.,0.,0.));
#4893=DIRECTION('center_axis',(0.,-1.,0.));
#4894=DIRECTION('ref_axis',(0.309016994374947,0.,-0.951056516295154));
#4895=DIRECTION('center_axis',(0.,-1.,0.));
#4896=DIRECTION('ref_axis',(1.,0.,0.));
#4897=DIRECTION('',(0.951056516295154,0.,0.309016994374947));
#4898=DIRECTION('center_axis',(0.,1.,0.));
#4899=DIRECTION('ref_axis',(1.,0.,0.));
#4900=DIRECTION('center_axis',(0.,-1.,0.));
#4901=DIRECTION('ref_axis',(0.309016994374947,0.,-0.951056516295154));
#4902=DIRECTION('center_axis',(0.,-1.,0.));
#4903=DIRECTION('ref_axis',(1.,0.,0.));
#4904=DIRECTION('',(0.809016994374947,0.,0.587785252292473));
#4905=DIRECTION('center_axis',(0.,1.,0.));
#4906=DIRECTION('ref_axis',(1.,0.,0.));
#4907=DIRECTION('center_axis',(0.,-1.,0.));
#4908=DIRECTION('ref_axis',(0.309016994374947,0.,-0.951056516295154));
#4909=DIRECTION('center_axis',(0.,-1.,0.));
#4910=DIRECTION('ref_axis',(1.,0.,0.));
#4911=DIRECTION('',(0.587785252292473,0.,0.809016994374947));
#4912=DIRECTION('center_axis',(0.,1.,0.));
#4913=DIRECTION('ref_axis',(1.,0.,0.));
#4914=DIRECTION('center_axis',(0.,-1.,0.));
#4915=DIRECTION('ref_axis',(0.309016994374947,0.,-0.951056516295154));
#4916=DIRECTION('center_axis',(0.,-1.,0.));
#4917=DIRECTION('ref_axis',(1.,0.,0.));
#4918=DIRECTION('',(1.66533453693773E-16,0.,1.));
#4919=DIRECTION('center_axis',(0.,1.,0.));
#4920=DIRECTION('ref_axis',(1.,0.,0.));
#4921=DIRECTION('center_axis',(0.,-1.,0.));
#4922=DIRECTION('ref_axis',(0.309016994374947,0.,-0.951056516295154));
#4923=DIRECTION('center_axis',(0.,-1.,0.));
#4924=DIRECTION('ref_axis',(1.,0.,0.));
#4925=DIRECTION('',(-0.309016994374947,0.,0.951056516295154));
#4926=DIRECTION('center_axis',(0.,1.,0.));
#4927=DIRECTION('ref_axis',(1.,0.,0.));
#4928=DIRECTION('center_axis',(0.,-1.,0.));
#4929=DIRECTION('ref_axis',(0.309016994374947,0.,-0.951056516295154));
#4930=DIRECTION('center_axis',(0.,-1.,0.));
#4931=DIRECTION('ref_axis',(1.,0.,0.));
#4932=DIRECTION('',(-0.587785252292473,0.,0.809016994374947));
#4933=DIRECTION('center_axis',(0.,1.,0.));
#4934=DIRECTION('ref_axis',(1.,0.,0.));
#4935=DIRECTION('center_axis',(0.,-1.,0.));
#4936=DIRECTION('ref_axis',(0.309016994374947,0.,-0.951056516295154));
#4937=DIRECTION('center_axis',(0.,-1.,0.));
#4938=DIRECTION('ref_axis',(1.,0.,0.));
#4939=DIRECTION('',(-0.809016994374947,0.,0.587785252292473));
#4940=DIRECTION('center_axis',(0.,1.,0.));
#4941=DIRECTION('ref_axis',(1.,0.,0.));
#4942=DIRECTION('center_axis',(0.,-1.,0.));
#4943=DIRECTION('ref_axis',(0.309016994374947,0.,-0.951056516295154));
#4944=DIRECTION('center_axis',(0.,-1.,0.));
#4945=DIRECTION('ref_axis',(1.,0.,0.));
#4946=DIRECTION('',(-0.951056516295153,0.,0.309016994374948));
#4947=DIRECTION('center_axis',(0.,1.,0.));
#4948=DIRECTION('ref_axis',(1.,0.,0.));
#4949=DIRECTION('center_axis',(0.,-1.,0.));
#4950=DIRECTION('ref_axis',(0.309016994374947,0.,-0.951056516295154));
#4951=DIRECTION('center_axis',(0.,-1.,0.));
#4952=DIRECTION('ref_axis',(1.,0.,0.));
#4953=DIRECTION('',(0.309016994374948,0.,0.951056516295154));
#4954=DIRECTION('center_axis',(0.,1.,0.));
#4955=DIRECTION('ref_axis',(1.,0.,0.));
#4956=DIRECTION('center_axis',(-0.951056516295154,0.,-0.309016994374947));
#4957=DIRECTION('ref_axis',(0.309016994374947,0.,-0.951056516295154));
#4958=DIRECTION('',(0.,1.,0.));
#4959=DIRECTION('',(-0.309016994374947,0.,0.951056516295154));
#4960=DIRECTION('',(0.,-1.,0.));
#4961=DIRECTION('center_axis',(1.,0.,-1.66533453693773E-16));
#4962=DIRECTION('ref_axis',(1.66533453693773E-16,0.,1.));
#4963=DIRECTION('',(0.,1.,0.));
#4964=DIRECTION('',(-1.66533453693773E-16,0.,-1.));
#4965=DIRECTION('',(0.,-1.,0.));
#4966=DIRECTION('center_axis',(0.951056516295154,0.,0.309016994374947));
#4967=DIRECTION('ref_axis',(-0.309016994374947,0.,0.951056516295154));
#4968=DIRECTION('',(0.,1.,0.));
#4969=DIRECTION('',(0.309016994374947,0.,-0.951056516295154));
#4970=DIRECTION('',(0.,-1.,0.));
#4971=DIRECTION('center_axis',(-0.951056516295154,0.,0.309016994374948));
#4972=DIRECTION('ref_axis',(-0.309016994374948,0.,-0.951056516295154));
#4973=DIRECTION('',(0.,1.,0.));
#4974=DIRECTION('',(0.309016994374948,0.,0.951056516295154));
#4975=DIRECTION('',(0.,-1.,0.));
#4976=DIRECTION('center_axis',(0.951056516295154,0.,-0.309016994374948));
#4977=DIRECTION('ref_axis',(0.309016994374948,0.,0.951056516295154));
#4978=DIRECTION('',(0.,1.,0.));
#4979=DIRECTION('',(-0.309016994374948,0.,-0.951056516295154));
#4980=DIRECTION('',(0.,-1.,0.));
#4981=DIRECTION('center_axis',(0.809016994374947,0.,-0.587785252292473));
#4982=DIRECTION('ref_axis',(0.587785252292473,0.,0.809016994374947));
#4983=DIRECTION('',(0.,1.,0.));
#4984=DIRECTION('',(-0.587785252292473,0.,-0.809016994374947));
#4985=DIRECTION('',(0.,-1.,0.));
#4986=DIRECTION('center_axis',(-0.809016994374947,0.,0.587785252292473));
#4987=DIRECTION('ref_axis',(-0.587785252292473,0.,-0.809016994374947));
#4988=DIRECTION('',(0.,1.,0.));
#4989=DIRECTION('',(0.587785252292473,0.,0.809016994374947));
#4990=DIRECTION('',(0.,-1.,0.));
#4991=DIRECTION('center_axis',(-0.587785252292473,0.,0.809016994374947));
#4992=DIRECTION('ref_axis',(-0.809016994374947,0.,-0.587785252292473));
#4993=DIRECTION('',(0.,1.,0.));
#4994=DIRECTION('',(0.809016994374947,0.,0.587785252292473));
#4995=DIRECTION('',(0.,-1.,0.));
#4996=DIRECTION('center_axis',(0.587785252292473,0.,-0.809016994374947));
#4997=DIRECTION('ref_axis',(0.809016994374947,0.,0.587785252292473));
#4998=DIRECTION('',(0.,1.,0.));
#4999=DIRECTION('',(-0.809016994374947,0.,-0.587785252292473));
#5000=DIRECTION('',(0.,-1.,0.));
#5001=DIRECTION('center_axis',(0.309016994374947,0.,-0.951056516295154));
#5002=DIRECTION('ref_axis',(0.951056516295154,0.,0.309016994374947));
#5003=DIRECTION('',(0.,1.,0.));
#5004=DIRECTION('',(-0.951056516295154,0.,-0.309016994374947));
#5005=DIRECTION('',(0.,-1.,0.));
#5006=DIRECTION('center_axis',(-0.309016994374947,0.,0.951056516295154));
#5007=DIRECTION('ref_axis',(-0.951056516295154,0.,-0.309016994374947));
#5008=DIRECTION('',(0.,1.,0.));
#5009=DIRECTION('',(0.951056516295154,0.,0.309016994374947));
#5010=DIRECTION('',(0.,-1.,0.));
#5011=DIRECTION('center_axis',(5.55111512312578E-17,0.,1.));
#5012=DIRECTION('ref_axis',(-1.,0.,5.55111512312578E-17));
#5013=DIRECTION('',(0.,1.,0.));
#5014=DIRECTION('',(1.,0.,-5.55111512312578E-17));
#5015=DIRECTION('',(0.,-1.,0.));
#5016=DIRECTION('center_axis',(-1.11022302462516E-16,0.,-1.));
#5017=DIRECTION('ref_axis',(1.,0.,-1.11022302462516E-16));
#5018=DIRECTION('',(0.,1.,0.));
#5019=DIRECTION('',(-1.,0.,1.11022302462516E-16));
#5020=DIRECTION('',(0.,-1.,0.));
#5021=DIRECTION('center_axis',(-0.309016994374948,0.,-0.951056516295154));
#5022=DIRECTION('ref_axis',(0.951056516295154,0.,-0.309016994374948));
#5023=DIRECTION('',(0.,1.,0.));
#5024=DIRECTION('',(-0.951056516295154,0.,0.309016994374948));
#5025=DIRECTION('',(0.,-1.,0.));
#5026=DIRECTION('center_axis',(0.309016994374948,0.,0.951056516295154));
#5027=DIRECTION('ref_axis',(-0.951056516295154,0.,0.309016994374948));
#5028=DIRECTION('',(0.,1.,0.));
#5029=DIRECTION('',(0.951056516295154,0.,-0.309016994374948));
#5030=DIRECTION('',(0.,-1.,0.));
#5031=DIRECTION('center_axis',(0.587785252292473,0.,0.809016994374947));
#5032=DIRECTION('ref_axis',(-0.809016994374947,0.,0.587785252292473));
#5033=DIRECTION('',(0.,1.,0.));
#5034=DIRECTION('',(0.809016994374947,0.,-0.587785252292473));
#5035=DIRECTION('',(0.,-1.,0.));
#5036=DIRECTION('center_axis',(-0.587785252292473,0.,-0.809016994374947));
#5037=DIRECTION('ref_axis',(0.809016994374947,0.,-0.587785252292473));
#5038=DIRECTION('',(0.,1.,0.));
#5039=DIRECTION('',(-0.809016994374947,0.,0.587785252292473));
#5040=DIRECTION('',(0.,-1.,0.));
#5041=DIRECTION('center_axis',(0.809016994374948,0.,0.587785252292473));
#5042=DIRECTION('ref_axis',(-0.587785252292473,0.,0.809016994374947));
#5043=DIRECTION('',(0.,1.,0.));
#5044=DIRECTION('',(0.587785252292473,0.,-0.809016994374947));
#5045=DIRECTION('',(0.,-1.,0.));
#5046=DIRECTION('center_axis',(-0.809016994374948,0.,-0.587785252292473));
#5047=DIRECTION('ref_axis',(0.587785252292473,0.,-0.809016994374947));
#5048=DIRECTION('',(0.,1.,0.));
#5049=DIRECTION('',(-0.587785252292473,0.,0.809016994374947));
#5050=DIRECTION('',(0.,-1.,0.));
#5051=DIRECTION('center_axis',(0.,1.,0.));
#5052=DIRECTION('ref_axis',(1.,0.,0.));
#5053=DIRECTION('center_axis',(0.,-1.,0.));
#5054=DIRECTION('ref_axis',(1.,0.,0.));
#5055=DIRECTION('',(0.,-1.,0.));
#5056=DIRECTION('center_axis',(0.,-1.,0.));
#5057=DIRECTION('ref_axis',(1.,0.,0.));
#5058=DIRECTION('center_axis',(0.,-1.,0.));
#5059=DIRECTION('ref_axis',(1.,0.,0.));
#5060=DIRECTION('center_axis',(0.,-1.,0.));
#5061=DIRECTION('ref_axis',(1.,0.,0.));
#5062=DIRECTION('center_axis',(0.,-1.,0.));
#5063=DIRECTION('ref_axis',(1.,0.,0.));
#5064=DIRECTION('center_axis',(0.,-1.,0.));
#5065=DIRECTION('ref_axis',(1.,0.,0.));
#5066=DIRECTION('',(0.,1.,0.));
#5067=DIRECTION('center_axis',(0.,-1.,0.));
#5068=DIRECTION('ref_axis',(1.,0.,0.));
#5069=DIRECTION('',(0.,-1.,0.));
#5070=DIRECTION('center_axis',(0.,-1.,0.));
#5071=DIRECTION('ref_axis',(1.,0.,0.));
#5072=DIRECTION('center_axis',(0.,-1.,0.));
#5073=DIRECTION('ref_axis',(1.,0.,0.));
#5074=DIRECTION('center_axis',(0.,-1.,0.));
#5075=DIRECTION('ref_axis',(1.,0.,0.));
#5076=DIRECTION('center_axis',(0.,-1.,0.));
#5077=DIRECTION('ref_axis',(1.,0.,0.));
#5078=DIRECTION('center_axis',(0.,-1.,0.));
#5079=DIRECTION('ref_axis',(1.,0.,0.));
#5080=DIRECTION('center_axis',(0.,-1.,0.));
#5081=DIRECTION('ref_axis',(1.,0.,0.));
#5082=DIRECTION('center_axis',(0.,-1.,0.));
#5083=DIRECTION('ref_axis',(1.,0.,0.));
#5084=DIRECTION('center_axis',(0.,-1.,0.));
#5085=DIRECTION('ref_axis',(1.,0.,0.));
#5086=DIRECTION('center_axis',(0.,-1.,0.));
#5087=DIRECTION('ref_axis',(1.,0.,0.));
#5088=DIRECTION('center_axis',(0.,-1.,0.));
#5089=DIRECTION('ref_axis',(1.,0.,0.));
#5090=DIRECTION('center_axis',(0.,-1.,0.));
#5091=DIRECTION('ref_axis',(1.,0.,0.));
#5092=DIRECTION('center_axis',(0.,-1.,0.));
#5093=DIRECTION('ref_axis',(1.,0.,0.));
#5094=DIRECTION('center_axis',(0.,-1.,0.));
#5095=DIRECTION('ref_axis',(1.,0.,0.));
#5096=DIRECTION('center_axis',(0.,-1.,0.));
#5097=DIRECTION('ref_axis',(1.,0.,0.));
#5098=DIRECTION('center_axis',(0.,-1.,0.));
#5099=DIRECTION('ref_axis',(1.,0.,0.));
#5100=DIRECTION('center_axis',(0.,1.,0.));
#5101=DIRECTION('ref_axis',(1.,0.,0.));
#5102=DIRECTION('center_axis',(0.,1.,0.));
#5103=DIRECTION('ref_axis',(1.,0.,0.));
#5104=DIRECTION('',(5.02869919278543E-17,0.,1.));
#5105=DIRECTION('center_axis',(0.,1.,0.));
#5106=DIRECTION('ref_axis',(1.,0.,0.));
#5107=DIRECTION('center_axis',(0.,1.,0.));
#5108=DIRECTION('ref_axis',(1.,0.,0.));
#5109=DIRECTION('center_axis',(0.,1.,0.));
#5110=DIRECTION('ref_axis',(1.,0.,0.));
#5111=DIRECTION('center_axis',(0.,1.,0.));
#5112=DIRECTION('ref_axis',(1.,0.,0.));
#5113=DIRECTION('center_axis',(0.,1.,0.));
#5114=DIRECTION('ref_axis',(1.,0.,0.));
#5115=DIRECTION('center_axis',(0.,1.,0.));
#5116=DIRECTION('ref_axis',(1.,0.,0.));
#5117=DIRECTION('center_axis',(0.,1.,0.));
#5118=DIRECTION('ref_axis',(1.,0.,0.));
#5119=DIRECTION('center_axis',(0.,1.,0.));
#5120=DIRECTION('ref_axis',(1.,0.,0.));
#5121=DIRECTION('center_axis',(0.,1.,0.));
#5122=DIRECTION('ref_axis',(1.,0.,0.));
#5123=DIRECTION('center_axis',(0.,1.,0.));
#5124=DIRECTION('ref_axis',(1.,0.,0.));
#5125=DIRECTION('center_axis',(0.,1.,0.));
#5126=DIRECTION('ref_axis',(1.,0.,0.));
#5127=DIRECTION('',(0.,0.,-1.));
#5128=DIRECTION('center_axis',(0.,1.,0.));
#5129=DIRECTION('ref_axis',(1.,0.,0.));
#5130=DIRECTION('center_axis',(0.,1.,0.));
#5131=DIRECTION('ref_axis',(1.,0.,0.));
#5132=DIRECTION('center_axis',(0.,1.,0.));
#5133=DIRECTION('ref_axis',(1.,0.,0.));
#5134=DIRECTION('center_axis',(0.,1.,0.));
#5135=DIRECTION('ref_axis',(1.,0.,0.));
#5136=DIRECTION('center_axis',(0.,1.,0.));
#5137=DIRECTION('ref_axis',(1.,0.,0.));
#5138=DIRECTION('center_axis',(0.,1.,0.));
#5139=DIRECTION('ref_axis',(1.,0.,0.));
#5140=DIRECTION('center_axis',(0.,1.,0.));
#5141=DIRECTION('ref_axis',(1.,0.,0.));
#5142=DIRECTION('center_axis',(0.,1.,0.));
#5143=DIRECTION('ref_axis',(1.,0.,0.));
#5144=DIRECTION('center_axis',(0.,1.,0.));
#5145=DIRECTION('ref_axis',(1.,0.,0.));
#5146=DIRECTION('center_axis',(0.,1.,0.));
#5147=DIRECTION('ref_axis',(1.,0.,0.));
#5148=DIRECTION('center_axis',(0.,1.,0.));
#5149=DIRECTION('ref_axis',(1.,0.,0.));
#5150=DIRECTION('center_axis',(0.,1.,0.));
#5151=DIRECTION('ref_axis',(1.,0.,0.));
#5152=DIRECTION('center_axis',(0.,1.,0.));
#5153=DIRECTION('ref_axis',(1.,0.,0.));
#5154=DIRECTION('center_axis',(0.,1.,0.));
#5155=DIRECTION('ref_axis',(1.,0.,0.));
#5156=DIRECTION('center_axis',(0.,1.,0.));
#5157=DIRECTION('ref_axis',(1.,0.,0.));
#5158=DIRECTION('center_axis',(0.,1.,0.));
#5159=DIRECTION('ref_axis',(1.,0.,0.));
#5160=DIRECTION('center_axis',(0.,1.,0.));
#5161=DIRECTION('ref_axis',(1.,0.,0.));
#5162=DIRECTION('center_axis',(0.,1.,0.));
#5163=DIRECTION('ref_axis',(1.,0.,0.));
#5164=DIRECTION('center_axis',(0.,1.,0.));
#5165=DIRECTION('ref_axis',(1.,0.,0.));
#5166=DIRECTION('center_axis',(0.,1.,0.));
#5167=DIRECTION('ref_axis',(1.,0.,0.));
#5168=DIRECTION('center_axis',(0.,1.,0.));
#5169=DIRECTION('ref_axis',(1.,0.,0.));
#5170=DIRECTION('center_axis',(0.,1.,0.));
#5171=DIRECTION('ref_axis',(1.,0.,0.));
#5172=DIRECTION('center_axis',(0.,1.,0.));
#5173=DIRECTION('ref_axis',(1.,0.,0.));
#5174=DIRECTION('center_axis',(0.,1.,0.));
#5175=DIRECTION('ref_axis',(1.,0.,0.));
#5176=DIRECTION('center_axis',(0.,1.,0.));
#5177=DIRECTION('ref_axis',(1.,0.,0.));
#5178=DIRECTION('center_axis',(1.,0.,0.));
#5179=DIRECTION('ref_axis',(0.,0.,1.));
#5180=DIRECTION('',(0.,0.,1.));
#5181=DIRECTION('',(0.,1.,0.));
#5182=DIRECTION('center_axis',(0.,-1.,0.));
#5183=DIRECTION('ref_axis',(0.,0.,-1.));
#5184=DIRECTION('',(-5.02869919278543E-17,0.,-1.));
#5185=DIRECTION('center_axis',(0.,1.,0.));
#5186=DIRECTION('ref_axis',(1.,0.,0.));
#5187=DIRECTION('center_axis',(-1.,0.,5.02869919278543E-17));
#5188=DIRECTION('ref_axis',(-5.02869919278543E-17,0.,-1.));
#5189=DIRECTION('',(0.,-1.,0.));
#5190=DIRECTION('center_axis',(0.,1.,0.));
#5191=DIRECTION('ref_axis',(1.,0.,0.));
#5192=DIRECTION('center_axis',(0.,1.,0.));
#5193=DIRECTION('ref_axis',(1.,0.,0.));
#5194=DIRECTION('',(0.,-1.,0.));
#5195=DIRECTION('center_axis',(0.,1.,0.));
#5196=DIRECTION('ref_axis',(1.,0.,0.));
#5197=DIRECTION('center_axis',(0.,1.,0.));
#5198=DIRECTION('ref_axis',(1.,0.,0.));
#5199=DIRECTION('center_axis',(0.,1.,0.));
#5200=DIRECTION('ref_axis',(1.,0.,0.));
#5201=DIRECTION('axis',(0.,0.,1.));
#5202=DIRECTION('refdir',(1.,0.,0.));
#5203=DIRECTION('center_axis',(-1.,0.,1.11022302462516E-16));
#5204=DIRECTION('ref_axis',(1.11022302462516E-16,0.,1.));
#5205=DIRECTION('',(1.11022302462516E-16,0.,1.));
#5206=DIRECTION('',(0.,-1.,0.));
#5207=DIRECTION('',(-1.11022302462516E-16,0.,-1.));
#5208=DIRECTION('',(0.,1.,0.));
#5209=DIRECTION('center_axis',(0.707106781186548,0.,0.707106781186548));
#5210=DIRECTION('ref_axis',(0.707106781186548,0.,-0.707106781186548));
#5211=DIRECTION('',(0.707106781186548,0.,-0.707106781186548));
#5212=DIRECTION('',(0.,-1.,0.));
#5213=DIRECTION('',(-0.707106781186548,0.,0.707106781186548));
#5214=DIRECTION('',(0.,1.,0.));
#5215=DIRECTION('center_axis',(0.,1.,0.));
#5216=DIRECTION('ref_axis',(0.707106781186548,0.,0.707106781186548));
#5217=DIRECTION('center_axis',(0.,1.,0.));
#5218=DIRECTION('ref_axis',(0.707106781186547,0.,0.707106781186547));
#5219=DIRECTION('center_axis',(0.,-1.,0.));
#5220=DIRECTION('ref_axis',(0.707106781186548,0.,0.707106781186548));
#5221=DIRECTION('center_axis',(0.,1.,0.));
#5222=DIRECTION('ref_axis',(0.707106781186547,0.,0.707106781186547));
#5223=DIRECTION('center_axis',(0.,1.,0.));
#5224=DIRECTION('ref_axis',(0.707106781186548,0.,0.707106781186548));
#5225=DIRECTION('center_axis',(0.,-1.,0.));
#5226=DIRECTION('ref_axis',(0.707106781186547,0.,0.707106781186547));
#5227=DIRECTION('center_axis',(0.,-1.,0.));
#5228=DIRECTION('ref_axis',(0.707106781186547,0.,0.707106781186547));
#5229=DIRECTION('',(0.,1.,0.));
#5230=DIRECTION('center_axis',(0.,1.,0.));
#5231=DIRECTION('ref_axis',(0.707106781186548,0.,0.707106781186548));
#5232=DIRECTION('center_axis',(0.,-1.,0.));
#5233=DIRECTION('ref_axis',(0.707106781186548,0.,0.707106781186548));
#5234=DIRECTION('center_axis',(0.,-1.,0.));
#5235=DIRECTION('ref_axis',(0.707106781186548,0.,0.707106781186548));
#5236=DIRECTION('',(0.,1.,0.));
#5237=DIRECTION('center_axis',(0.,1.,0.));
#5238=DIRECTION('ref_axis',(0.707106781186548,0.,0.707106781186548));
#5239=DIRECTION('center_axis',(0.,1.,0.));
#5240=DIRECTION('ref_axis',(0.707106781186548,0.,0.707106781186548));
#5241=DIRECTION('center_axis',(0.,-1.,0.));
#5242=DIRECTION('ref_axis',(0.707106781186548,0.,0.707106781186548));
#5243=DIRECTION('center_axis',(0.,1.,0.));
#5244=DIRECTION('ref_axis',(0.707106781186547,0.,0.707106781186547));
#5245=DIRECTION('center_axis',(0.,1.,0.));
#5246=DIRECTION('ref_axis',(0.707106781186547,0.,0.707106781186547));
#5247=DIRECTION('center_axis',(0.,1.,0.));
#5248=DIRECTION('ref_axis',(0.707106781186548,0.,0.707106781186548));
#5249=DIRECTION('axis',(0.,0.,1.));
#5250=DIRECTION('refdir',(1.,0.,0.));
#5251=DIRECTION('center_axis',(-0.707106781186548,0.,-0.707106781186547));
#5252=DIRECTION('ref_axis',(-0.707106781186547,0.,0.707106781186548));
#5253=DIRECTION('',(-0.707106781186547,0.,0.707106781186548));
#5254=DIRECTION('',(0.,-1.,0.));
#5255=DIRECTION('',(0.707106781186547,0.,-0.707106781186548));
#5256=DIRECTION('',(0.,1.,0.));
#5257=DIRECTION('center_axis',(6.12323399573677E-17,0.,1.));
#5258=DIRECTION('ref_axis',(1.,0.,-6.12323399573677E-17));
#5259=DIRECTION('',(1.,0.,-6.12323399573677E-17));
#5260=DIRECTION('',(0.,-1.,0.));
#5261=DIRECTION('',(-1.,0.,6.12323399573677E-17));
#5262=DIRECTION('',(0.,1.,0.));
#5263=DIRECTION('center_axis',(0.,1.,0.));
#5264=DIRECTION('ref_axis',(6.12323399573677E-17,0.,1.));
#5265=DIRECTION('center_axis',(0.,1.,0.));
#5266=DIRECTION('ref_axis',(6.12323399573677E-17,0.,1.));
#5267=DIRECTION('center_axis',(0.,-1.,0.));
#5268=DIRECTION('ref_axis',(6.12323399573676E-17,0.,1.));
#5269=DIRECTION('center_axis',(0.,1.,0.));
#5270=DIRECTION('ref_axis',(6.12323399573677E-17,0.,1.));
#5271=DIRECTION('center_axis',(0.,1.,0.));
#5272=DIRECTION('ref_axis',(6.12323399573677E-17,0.,1.));
#5273=DIRECTION('center_axis',(0.,-1.,0.));
#5274=DIRECTION('ref_axis',(6.12323399573677E-17,0.,1.));
#5275=DIRECTION('center_axis',(0.,-1.,0.));
#5276=DIRECTION('ref_axis',(6.12323399573677E-17,0.,1.));
#5277=DIRECTION('',(0.,1.,0.));
#5278=DIRECTION('center_axis',(0.,1.,0.));
#5279=DIRECTION('ref_axis',(6.12323399573677E-17,0.,1.));
#5280=DIRECTION('center_axis',(0.,-1.,0.));
#5281=DIRECTION('ref_axis',(6.12323399573677E-17,0.,1.));
#5282=DIRECTION('center_axis',(0.,-1.,0.));
#5283=DIRECTION('ref_axis',(6.12323399573677E-17,0.,1.));
#5284=DIRECTION('',(0.,1.,0.));
#5285=DIRECTION('center_axis',(0.,1.,0.));
#5286=DIRECTION('ref_axis',(6.12323399573677E-17,0.,1.));
#5287=DIRECTION('center_axis',(0.,1.,0.));
#5288=DIRECTION('ref_axis',(6.12323399573676E-17,0.,1.));
#5289=DIRECTION('center_axis',(0.,-1.,0.));
#5290=DIRECTION('ref_axis',(6.12323399573676E-17,0.,1.));
#5291=DIRECTION('center_axis',(0.,1.,0.));
#5292=DIRECTION('ref_axis',(6.12323399573677E-17,0.,1.));
#5293=DIRECTION('center_axis',(0.,1.,0.));
#5294=DIRECTION('ref_axis',(6.12323399573677E-17,0.,1.));
#5295=DIRECTION('center_axis',(0.,1.,0.));
#5296=DIRECTION('ref_axis',(6.12323399573677E-17,0.,1.));
#5297=DIRECTION('axis',(0.,0.,1.));
#5298=DIRECTION('refdir',(1.,0.,0.));
#5299=DIRECTION('center_axis',(0.707106781186547,0.,-0.707106781186548));
#5300=DIRECTION('ref_axis',(-0.707106781186548,0.,-0.707106781186547));
#5301=DIRECTION('',(-0.707106781186548,0.,-0.707106781186547));
#5302=DIRECTION('',(0.,-1.,0.));
#5303=DIRECTION('',(0.707106781186548,0.,0.707106781186547));
#5304=DIRECTION('',(0.,1.,0.));
#5305=DIRECTION('center_axis',(-1.,0.,1.22464679914735E-16));
#5306=DIRECTION('ref_axis',(1.22464679914735E-16,0.,1.));
#5307=DIRECTION('',(1.22464679914735E-16,0.,1.));
#5308=DIRECTION('',(0.,-1.,0.));
#5309=DIRECTION('',(-1.22464679914735E-16,0.,-1.));
#5310=DIRECTION('',(0.,1.,0.));
#5311=DIRECTION('center_axis',(0.,1.,0.));
#5312=DIRECTION('ref_axis',(-1.,0.,1.22464679914735E-16));
#5313=DIRECTION('center_axis',(0.,1.,0.));
#5314=DIRECTION('ref_axis',(-1.,0.,1.22464679914735E-16));
#5315=DIRECTION('center_axis',(0.,-1.,0.));
#5316=DIRECTION('ref_axis',(-1.,0.,1.22464679914735E-16));
#5317=DIRECTION('center_axis',(0.,1.,0.));
#5318=DIRECTION('ref_axis',(-1.,0.,1.22464679914735E-16));
#5319=DIRECTION('center_axis',(0.,1.,0.));
#5320=DIRECTION('ref_axis',(-1.,0.,1.22464679914735E-16));
#5321=DIRECTION('center_axis',(0.,-1.,0.));
#5322=DIRECTION('ref_axis',(-1.,0.,1.22464679914735E-16));
#5323=DIRECTION('center_axis',(0.,-1.,0.));
#5324=DIRECTION('ref_axis',(-1.,0.,1.22464679914735E-16));
#5325=DIRECTION('',(0.,1.,0.));
#5326=DIRECTION('center_axis',(0.,1.,0.));
#5327=DIRECTION('ref_axis',(-1.,0.,1.22464679914735E-16));
#5328=DIRECTION('center_axis',(0.,-1.,0.));
#5329=DIRECTION('ref_axis',(-1.,0.,1.22464679914735E-16));
#5330=DIRECTION('center_axis',(0.,-1.,0.));
#5331=DIRECTION('ref_axis',(-1.,0.,1.22464679914735E-16));
#5332=DIRECTION('',(0.,1.,0.));
#5333=DIRECTION('center_axis',(0.,1.,0.));
#5334=DIRECTION('ref_axis',(-1.,0.,1.22464679914735E-16));
#5335=DIRECTION('center_axis',(0.,1.,0.));
#5336=DIRECTION('ref_axis',(-1.,0.,1.22464679914735E-16));
#5337=DIRECTION('center_axis',(0.,-1.,0.));
#5338=DIRECTION('ref_axis',(-1.,0.,1.22464679914735E-16));
#5339=DIRECTION('center_axis',(0.,1.,0.));
#5340=DIRECTION('ref_axis',(-1.,0.,1.22464679914735E-16));
#5341=DIRECTION('center_axis',(0.,1.,0.));
#5342=DIRECTION('ref_axis',(-1.,0.,1.22464679914735E-16));
#5343=DIRECTION('center_axis',(0.,1.,0.));
#5344=DIRECTION('ref_axis',(-1.,0.,1.22464679914735E-16));
#5345=DIRECTION('axis',(0.,0.,1.));
#5346=DIRECTION('refdir',(1.,0.,0.));
#5347=DIRECTION('center_axis',(1.,0.,-3.33066907387547E-16));
#5348=DIRECTION('ref_axis',(-3.33066907387547E-16,0.,-1.));
#5349=DIRECTION('',(-3.33066907387547E-16,0.,-1.));
#5350=DIRECTION('',(0.,-1.,0.));
#5351=DIRECTION('',(3.33066907387547E-16,0.,1.));
#5352=DIRECTION('',(0.,1.,0.));
#5353=DIRECTION('center_axis',(-0.707106781186548,0.,-0.707106781186547));
#5354=DIRECTION('ref_axis',(-0.707106781186547,0.,0.707106781186548));
#5355=DIRECTION('',(-0.707106781186547,0.,0.707106781186548));
#5356=DIRECTION('',(0.,-1.,0.));
#5357=DIRECTION('',(0.707106781186547,0.,-0.707106781186548));
#5358=DIRECTION('',(0.,1.,0.));
#5359=DIRECTION('center_axis',(0.,1.,0.));
#5360=DIRECTION('ref_axis',(-0.707106781186548,0.,-0.707106781186547));
#5361=DIRECTION('center_axis',(0.,1.,0.));
#5362=DIRECTION('ref_axis',(-0.707106781186548,0.,-0.707106781186547));
#5363=DIRECTION('center_axis',(0.,-1.,0.));
#5364=DIRECTION('ref_axis',(-0.707106781186548,0.,-0.707106781186547));
#5365=DIRECTION('center_axis',(0.,1.,0.));
#5366=DIRECTION('ref_axis',(-0.707106781186547,0.,-0.707106781186547));
#5367=DIRECTION('center_axis',(0.,1.,0.));
#5368=DIRECTION('ref_axis',(-0.707106781186548,0.,-0.707106781186547));
#5369=DIRECTION('center_axis',(0.,-1.,0.));
#5370=DIRECTION('ref_axis',(-0.707106781186547,0.,-0.707106781186547));
#5371=DIRECTION('center_axis',(0.,-1.,0.));
#5372=DIRECTION('ref_axis',(-0.707106781186547,0.,-0.707106781186547));
#5373=DIRECTION('',(0.,1.,0.));
#5374=DIRECTION('center_axis',(0.,1.,0.));
#5375=DIRECTION('ref_axis',(-0.707106781186548,0.,-0.707106781186547));
#5376=DIRECTION('center_axis',(0.,-1.,0.));
#5377=DIRECTION('ref_axis',(-0.707106781186548,0.,-0.707106781186547));
#5378=DIRECTION('center_axis',(0.,-1.,0.));
#5379=DIRECTION('ref_axis',(-0.707106781186548,0.,-0.707106781186547));
#5380=DIRECTION('',(0.,1.,0.));
#5381=DIRECTION('center_axis',(0.,1.,0.));
#5382=DIRECTION('ref_axis',(-0.707106781186548,0.,-0.707106781186547));
#5383=DIRECTION('center_axis',(0.,1.,0.));
#5384=DIRECTION('ref_axis',(-0.707106781186548,0.,-0.707106781186547));
#5385=DIRECTION('center_axis',(0.,-1.,0.));
#5386=DIRECTION('ref_axis',(-0.707106781186548,0.,-0.707106781186547));
#5387=DIRECTION('center_axis',(0.,1.,0.));
#5388=DIRECTION('ref_axis',(-0.707106781186548,0.,-0.707106781186547));
#5389=DIRECTION('center_axis',(0.,1.,0.));
#5390=DIRECTION('ref_axis',(-0.707106781186548,0.,-0.707106781186547));
#5391=DIRECTION('center_axis',(0.,1.,0.));
#5392=DIRECTION('ref_axis',(-0.707106781186548,0.,-0.707106781186547));
#5393=DIRECTION('axis',(0.,0.,1.));
#5394=DIRECTION('refdir',(1.,0.,0.));
#5395=DIRECTION('center_axis',(0.707106781186548,0.,0.707106781186547));
#5396=DIRECTION('ref_axis',(0.707106781186547,0.,-0.707106781186548));
#5397=DIRECTION('',(0.707106781186547,0.,-0.707106781186548));
#5398=DIRECTION('',(0.,-1.,0.));
#5399=DIRECTION('',(-0.707106781186547,0.,0.707106781186548));
#5400=DIRECTION('',(0.,1.,0.));
#5401=DIRECTION('center_axis',(-1.83697019872103E-16,0.,-1.));
#5402=DIRECTION('ref_axis',(-1.,0.,1.83697019872103E-16));
#5403=DIRECTION('',(-1.,0.,1.83697019872103E-16));
#5404=DIRECTION('',(0.,-1.,0.));
#5405=DIRECTION('',(1.,0.,-1.83697019872103E-16));
#5406=DIRECTION('',(0.,1.,0.));
#5407=DIRECTION('center_axis',(0.,1.,0.));
#5408=DIRECTION('ref_axis',(-1.83697019872103E-16,0.,-1.));
#5409=DIRECTION('center_axis',(0.,1.,0.));
#5410=DIRECTION('ref_axis',(-1.83697019872103E-16,0.,-1.));
#5411=DIRECTION('center_axis',(0.,-1.,0.));
#5412=DIRECTION('ref_axis',(-1.83697019872103E-16,0.,-1.));
#5413=DIRECTION('center_axis',(0.,1.,0.));
#5414=DIRECTION('ref_axis',(-1.83697019872103E-16,0.,-1.));
#5415=DIRECTION('center_axis',(0.,1.,0.));
#5416=DIRECTION('ref_axis',(-1.83697019872103E-16,0.,-1.));
#5417=DIRECTION('center_axis',(0.,-1.,0.));
#5418=DIRECTION('ref_axis',(-1.83697019872103E-16,0.,-1.));
#5419=DIRECTION('center_axis',(0.,-1.,0.));
#5420=DIRECTION('ref_axis',(-1.83697019872103E-16,0.,-1.));
#5421=DIRECTION('',(0.,1.,0.));
#5422=DIRECTION('center_axis',(0.,1.,0.));
#5423=DIRECTION('ref_axis',(-1.83697019872103E-16,0.,-1.));
#5424=DIRECTION('center_axis',(0.,-1.,0.));
#5425=DIRECTION('ref_axis',(-1.83697019872103E-16,0.,-1.));
#5426=DIRECTION('center_axis',(0.,-1.,0.));
#5427=DIRECTION('ref_axis',(-1.83697019872103E-16,0.,-1.));
#5428=DIRECTION('',(0.,1.,0.));
#5429=DIRECTION('center_axis',(0.,1.,0.));
#5430=DIRECTION('ref_axis',(-1.83697019872103E-16,0.,-1.));
#5431=DIRECTION('center_axis',(0.,1.,0.));
#5432=DIRECTION('ref_axis',(-1.83697019872103E-16,0.,-1.));
#5433=DIRECTION('center_axis',(0.,-1.,0.));
#5434=DIRECTION('ref_axis',(-1.83697019872103E-16,0.,-1.));
#5435=DIRECTION('center_axis',(0.,1.,0.));
#5436=DIRECTION('ref_axis',(-1.83697019872103E-16,0.,-1.));
#5437=DIRECTION('center_axis',(0.,1.,0.));
#5438=DIRECTION('ref_axis',(-1.83697019872103E-16,0.,-1.));
#5439=DIRECTION('center_axis',(0.,1.,0.));
#5440=DIRECTION('ref_axis',(-1.83697019872103E-16,0.,-1.));
#5441=DIRECTION('axis',(0.,0.,1.));
#5442=DIRECTION('refdir',(1.,0.,0.));
#5443=DIRECTION('center_axis',(3.88578058618805E-16,0.,1.));
#5444=DIRECTION('ref_axis',(1.,0.,-3.88578058618805E-16));
#5445=DIRECTION('',(1.,0.,-3.88578058618805E-16));
#5446=DIRECTION('',(0.,-1.,0.));
#5447=DIRECTION('',(-1.,0.,3.88578058618805E-16));
#5448=DIRECTION('',(0.,1.,0.));
#5449=DIRECTION('center_axis',(0.707106781186547,0.,-0.707106781186548));
#5450=DIRECTION('ref_axis',(-0.707106781186548,0.,-0.707106781186547));
#5451=DIRECTION('',(-0.707106781186548,0.,-0.707106781186547));
#5452=DIRECTION('',(0.,-1.,0.));
#5453=DIRECTION('',(0.707106781186548,0.,0.707106781186547));
#5454=DIRECTION('',(0.,1.,0.));
#5455=DIRECTION('center_axis',(0.,1.,0.));
#5456=DIRECTION('ref_axis',(0.707106781186547,0.,-0.707106781186548));
#5457=DIRECTION('center_axis',(0.,1.,0.));
#5458=DIRECTION('ref_axis',(0.707106781186547,0.,-0.707106781186548));
#5459=DIRECTION('center_axis',(0.,-1.,0.));
#5460=DIRECTION('ref_axis',(0.707106781186547,0.,-0.707106781186548));
#5461=DIRECTION('center_axis',(0.,1.,0.));
#5462=DIRECTION('ref_axis',(0.707106781186547,0.,-0.707106781186548));
#5463=DIRECTION('center_axis',(0.,1.,0.));
#5464=DIRECTION('ref_axis',(0.707106781186547,0.,-0.707106781186548));
#5465=DIRECTION('center_axis',(0.,-1.,0.));
#5466=DIRECTION('ref_axis',(0.707106781186547,0.,-0.707106781186548));
#5467=DIRECTION('center_axis',(0.,-1.,0.));
#5468=DIRECTION('ref_axis',(0.707106781186547,0.,-0.707106781186548));
#5469=DIRECTION('',(0.,1.,0.));
#5470=DIRECTION('center_axis',(0.,1.,0.));
#5471=DIRECTION('ref_axis',(0.707106781186547,0.,-0.707106781186548));
#5472=DIRECTION('center_axis',(0.,-1.,0.));
#5473=DIRECTION('ref_axis',(0.707106781186547,0.,-0.707106781186548));
#5474=DIRECTION('center_axis',(0.,-1.,0.));
#5475=DIRECTION('ref_axis',(0.707106781186547,0.,-0.707106781186548));
#5476=DIRECTION('',(0.,1.,0.));
#5477=DIRECTION('center_axis',(0.,1.,0.));
#5478=DIRECTION('ref_axis',(0.707106781186547,0.,-0.707106781186548));
#5479=DIRECTION('center_axis',(0.,1.,0.));
#5480=DIRECTION('ref_axis',(0.707106781186547,0.,-0.707106781186548));
#5481=DIRECTION('center_axis',(0.,-1.,0.));
#5482=DIRECTION('ref_axis',(0.707106781186547,0.,-0.707106781186548));
#5483=DIRECTION('center_axis',(0.,1.,0.));
#5484=DIRECTION('ref_axis',(0.707106781186547,0.,-0.707106781186548));
#5485=DIRECTION('center_axis',(0.,1.,0.));
#5486=DIRECTION('ref_axis',(0.707106781186547,0.,-0.707106781186548));
#5487=DIRECTION('center_axis',(0.,1.,0.));
#5488=DIRECTION('ref_axis',(0.707106781186547,0.,-0.707106781186548));
#5489=DIRECTION('axis',(0.,0.,1.));
#5490=DIRECTION('refdir',(1.,0.,0.));
#5491=DIRECTION('center_axis',(-2.22044604925031E-16,0.,-1.));
#5492=DIRECTION('ref_axis',(-1.,0.,2.22044604925031E-16));
#5493=DIRECTION('',(-1.,0.,2.22044604925031E-16));
#5494=DIRECTION('',(0.,-1.,0.));
#5495=DIRECTION('',(1.,0.,-2.22044604925031E-16));
#5496=DIRECTION('',(0.,1.,0.));
#5497=DIRECTION('center_axis',(-0.707106781186547,0.,0.707106781186548));
#5498=DIRECTION('ref_axis',(0.707106781186548,0.,0.707106781186547));
#5499=DIRECTION('',(0.707106781186548,0.,0.707106781186547));
#5500=DIRECTION('',(0.,-1.,0.));
#5501=DIRECTION('',(-0.707106781186548,0.,-0.707106781186547));
#5502=DIRECTION('',(0.,1.,0.));
#5503=DIRECTION('center_axis',(0.,1.,0.));
#5504=DIRECTION('ref_axis',(-0.707106781186547,0.,0.707106781186548));
#5505=DIRECTION('center_axis',(0.,1.,0.));
#5506=DIRECTION('ref_axis',(-0.707106781186547,0.,0.707106781186548));
#5507=DIRECTION('center_axis',(0.,-1.,0.));
#5508=DIRECTION('ref_axis',(-0.707106781186547,0.,0.707106781186548));
#5509=DIRECTION('center_axis',(0.,1.,0.));
#5510=DIRECTION('ref_axis',(-0.707106781186547,0.,0.707106781186547));
#5511=DIRECTION('center_axis',(0.,1.,0.));
#5512=DIRECTION('ref_axis',(-0.707106781186547,0.,0.707106781186548));
#5513=DIRECTION('center_axis',(0.,-1.,0.));
#5514=DIRECTION('ref_axis',(-0.707106781186547,0.,0.707106781186547));
#5515=DIRECTION('center_axis',(0.,-1.,0.));
#5516=DIRECTION('ref_axis',(-0.707106781186547,0.,0.707106781186547));
#5517=DIRECTION('',(0.,1.,0.));
#5518=DIRECTION('center_axis',(0.,1.,0.));
#5519=DIRECTION('ref_axis',(-0.707106781186547,0.,0.707106781186548));
#5520=DIRECTION('center_axis',(0.,-1.,0.));
#5521=DIRECTION('ref_axis',(-0.707106781186547,0.,0.707106781186548));
#5522=DIRECTION('center_axis',(0.,-1.,0.));
#5523=DIRECTION('ref_axis',(-0.707106781186547,0.,0.707106781186548));
#5524=DIRECTION('',(0.,1.,0.));
#5525=DIRECTION('center_axis',(0.,1.,0.));
#5526=DIRECTION('ref_axis',(-0.707106781186547,0.,0.707106781186548));
#5527=DIRECTION('center_axis',(0.,1.,0.));
#5528=DIRECTION('ref_axis',(-0.707106781186547,0.,0.707106781186548));
#5529=DIRECTION('center_axis',(0.,-1.,0.));
#5530=DIRECTION('ref_axis',(-0.707106781186547,0.,0.707106781186548));
#5531=DIRECTION('center_axis',(0.,1.,0.));
#5532=DIRECTION('ref_axis',(-0.707106781186547,0.,0.707106781186548));
#5533=DIRECTION('center_axis',(0.,1.,0.));
#5534=DIRECTION('ref_axis',(-0.707106781186547,0.,0.707106781186548));
#5535=DIRECTION('center_axis',(0.,1.,0.));
#5536=DIRECTION('ref_axis',(-0.707106781186547,0.,0.707106781186548));
#5537=DIRECTION('',(0.,0.,1.));
#5538=DIRECTION('',(1.,0.,0.));
#5539=DIRECTION('',(0.,0.,1.));
#5540=DIRECTION('',(1.,0.,0.));
#5541=DIRECTION('',(0.,0.,1.));
#5542=DIRECTION('',(1.,0.,0.));
#5543=DIRECTION('',(0.,0.,1.));
#5544=DIRECTION('',(1.,0.,0.));
#5545=DIRECTION('',(0.,0.,1.));
#5546=DIRECTION('',(1.,0.,0.));
#5547=DIRECTION('',(0.,0.,1.));
#5548=DIRECTION('',(1.,0.,0.));
#5549=DIRECTION('',(0.,0.,1.));
#5550=DIRECTION('',(1.,0.,0.));
#5551=DIRECTION('',(0.,0.,1.));
#5552=DIRECTION('',(1.,0.,0.));
#5553=DIRECTION('',(0.,0.,1.));
#5554=DIRECTION('',(1.,0.,0.));
#5555=DIRECTION('',(0.,0.,1.));
#5556=DIRECTION('',(1.,0.,0.));
#5557=DIRECTION('',(0.,0.,1.));
#5558=DIRECTION('',(1.,0.,0.));
#5559=DIRECTION('',(0.,0.,1.));
#5560=DIRECTION('',(1.,0.,0.));
#5561=DIRECTION('',(0.,0.,1.));
#5562=DIRECTION('',(1.,0.,0.));
#5563=CARTESIAN_POINT('',(0.,0.,0.));
#5564=CARTESIAN_POINT('',(0.,0.,0.));
#5565=CARTESIAN_POINT('Origin',(0.,0.,114.33240815703));
#5566=CARTESIAN_POINT('',(-27.848517275114,-4.,135.532881868193));
#5567=CARTESIAN_POINT('',(-27.848517275114,2.,135.532881868193));
#5568=CARTESIAN_POINT('',(-27.848517275114,0.,135.532881868193));
#5569=CARTESIAN_POINT('',(-35.,-4.,114.33240815703));
#5570=CARTESIAN_POINT('Origin',(0.,-4.,114.33240815703));
#5571=CARTESIAN_POINT('',(-35.,3.,114.33240815703));
#5572=CARTESIAN_POINT('',(-35.,0.,114.33240815703));
#5573=CARTESIAN_POINT('Origin',(0.,3.,114.33240815703));
#5574=CARTESIAN_POINT('',(27.848517275114,-4.,135.532881868193));
#5575=CARTESIAN_POINT('Origin',(0.,-4.,114.33240815703));
#5576=CARTESIAN_POINT('',(27.848517275114,2.,135.532881868193));
#5577=CARTESIAN_POINT('',(27.848517275114,0.,135.532881868193));
#5578=CARTESIAN_POINT('Origin',(0.,2.,114.33240815703));
#5579=CARTESIAN_POINT('Origin',(0.,3.,114.33240815703));
#5580=CARTESIAN_POINT('',(-33.,3.,114.33240815703));
#5581=CARTESIAN_POINT('Origin',(0.,3.,114.33240815703));
#5582=CARTESIAN_POINT('Origin',(0.,-4.,114.33240815703));
#5583=CARTESIAN_POINT('',(-31.8268768858446,-4.,138.561520969787));
#5584=CARTESIAN_POINT('',(-13.924258637557,-4.,124.932645012611));
#5585=CARTESIAN_POINT('',(-40.,-4.,114.33240815703));
#5586=CARTESIAN_POINT('Origin',(0.,-4.,114.33240815703));
#5587=CARTESIAN_POINT('',(31.8268768858446,-4.,138.561520969787));
#5588=CARTESIAN_POINT('Origin',(0.,-4.,114.33240815703));
#5589=CARTESIAN_POINT('',(15.9134384429223,-4.,126.446964563409));
#5590=CARTESIAN_POINT('Origin',(31.8268768858446,0.,138.561520969787));
#5591=CARTESIAN_POINT('',(31.8268768858446,2.,138.561520969787));
#5592=CARTESIAN_POINT('',(31.8268768858446,0.,138.561520969787));
#5593=CARTESIAN_POINT('',(31.8268768858446,2.,138.561520969787));
#5594=CARTESIAN_POINT('Origin',(-27.848517275114,0.,135.532881868193));
#5595=CARTESIAN_POINT('',(-31.8268768858446,2.,138.561520969787));
#5596=CARTESIAN_POINT('',(-31.8268768858446,2.,138.561520969787));
#5597=CARTESIAN_POINT('',(-31.8268768858446,0.,138.561520969787));
#5598=CARTESIAN_POINT('Origin',(0.,2.,144.932645012611));
#5599=CARTESIAN_POINT('Origin',(0.,2.,114.33240815703));
#5600=CARTESIAN_POINT('Origin',(0.,0.,114.33240815703));
#5601=CARTESIAN_POINT('',(-33.,4.,114.33240815703));
#5602=CARTESIAN_POINT('Origin',(0.,4.,114.33240815703));
#5603=CARTESIAN_POINT('',(-33.,0.,114.33240815703));
#5604=CARTESIAN_POINT('Origin',(0.,0.,114.33240815703));
#5605=CARTESIAN_POINT('',(-40.,4.,114.33240815703));
#5606=CARTESIAN_POINT('Origin',(0.,4.,114.33240815703));
#5607=CARTESIAN_POINT('',(-40.,0.,114.33240815703));
#5608=CARTESIAN_POINT('Origin',(0.,4.,114.33240815703));
#5609=CARTESIAN_POINT('',(0.,0.,0.));
#5610=CARTESIAN_POINT('Origin',(-2.77555756156289E-16,0.75,164.85));
#5611=CARTESIAN_POINT('',(-1.25,0.75,164.85));
#5612=CARTESIAN_POINT('Origin',(-2.77555756156289E-16,0.75,164.85));
#5613=CARTESIAN_POINT('',(-3.54096181102999E-16,0.75,166.1));
#5614=CARTESIAN_POINT('Origin',(-2.77555756156289E-16,0.75,164.85));
#5615=CARTESIAN_POINT('Origin',(-2.77555756156289E-16,0.75,150.));
#5616=CARTESIAN_POINT('',(-1.25,0.75,159.));
#5617=CARTESIAN_POINT('',(-1.25,0.75,150.));
#5618=CARTESIAN_POINT('Origin',(-2.77555756156289E-16,0.75,159.));
#5619=CARTESIAN_POINT('Origin',(-2.77555756156289E-16,0.75,159.));
#5620=CARTESIAN_POINT('',(-0.75,0.75,159.));
#5621=CARTESIAN_POINT('Origin',(-2.77555756156289E-16,0.75,159.));
#5622=CARTESIAN_POINT('Origin',(-2.77555756156289E-16,0.75,150.));
#5623=CARTESIAN_POINT('',(-0.75,0.75,144.));
#5624=CARTESIAN_POINT('Origin',(-2.77555756156289E-16,0.75,144.));
#5625=CARTESIAN_POINT('',(-0.75,0.75,150.));
#5626=CARTESIAN_POINT('Origin',(-2.77555756156289E-16,0.75,144.));
#5627=CARTESIAN_POINT('',(0.,0.,0.));
#5628=CARTESIAN_POINT('Origin',(3.53553390593273,-3.,117.867942062963));
#5629=CARTESIAN_POINT('',(3.53553390593273,-3.,117.867942062963));
#5630=CARTESIAN_POINT('',(23.9002092041053,-3.,138.232617361136));
#5631=CARTESIAN_POINT('',(1.76776695296637,-3.,116.100175109997));
#5632=CARTESIAN_POINT('',(3.53553390593273,-2.9,117.867942062963));
#5633=CARTESIAN_POINT('',(3.53553390593273,-3.,117.867942062963));
#5634=CARTESIAN_POINT('',(23.9002092041053,-2.9,138.232617361136));
#5635=CARTESIAN_POINT('',(1.76776695296637,-2.9,116.100175109997));
#5636=CARTESIAN_POINT('',(23.9002092041053,-3.,138.232617361136));
#5637=CARTESIAN_POINT('Origin',(-2.22044604925031E-15,-3.,148.13240815703));
#5638=CARTESIAN_POINT('',(-2.22044604925031E-15,-3.,148.13240815703));
#5639=CARTESIAN_POINT('',(-2.22044604925031E-15,-3.,119.33240815703));
#5640=CARTESIAN_POINT('',(-2.22044604925031E-15,-3.,131.23240815703));
#5641=CARTESIAN_POINT('',(-2.22044604925031E-15,-2.9,148.13240815703));
#5642=CARTESIAN_POINT('',(-2.22044604925031E-15,-3.,148.13240815703));
#5643=CARTESIAN_POINT('',(-2.22044604925031E-15,-2.9,119.33240815703));
#5644=CARTESIAN_POINT('',(-2.22044604925031E-15,-2.9,131.23240815703));
#5645=CARTESIAN_POINT('',(-2.22044604925031E-15,-3.,119.33240815703));
#5646=CARTESIAN_POINT('Origin',(0.,-3.,114.33240815703));
#5647=CARTESIAN_POINT('Origin',(-2.22044604925031E-15,-3.,114.33240815703));
#5648=CARTESIAN_POINT('Origin',(-2.22044604925031E-15,-3.,114.33240815703));
#5649=CARTESIAN_POINT('',(5.20441727387071,-3.,142.877430577928));
#5650=CARTESIAN_POINT('Origin',(6.30441727387071,-3.,142.877430577928));
#5651=CARTESIAN_POINT('',(15.6482292407074,-3.,138.291974085347));
#5652=CARTESIAN_POINT('Origin',(16.7482292407074,-3.,138.291974085347));
#5653=CARTESIAN_POINT('Origin',(6.30441727387071,-3.,142.877430577928));
#5654=CARTESIAN_POINT('',(5.20441727387071,-3.5,142.877430577928));
#5655=CARTESIAN_POINT('Origin',(6.30441727387071,-3.5,142.877430577928));
#5656=CARTESIAN_POINT('',(5.20441727387071,-3.,142.877430577928));
#5657=CARTESIAN_POINT('Origin',(6.30441727387071,-3.5,142.877430577928));
#5658=CARTESIAN_POINT('Origin',(16.7482292407074,-3.,138.291974085347));
#5659=CARTESIAN_POINT('',(15.6482292407074,-3.5,138.291974085347));
#5660=CARTESIAN_POINT('Origin',(16.7482292407074,-3.5,138.291974085347));
#5661=CARTESIAN_POINT('',(15.6482292407074,-3.,138.291974085347));
#5662=CARTESIAN_POINT('Origin',(16.7482292407074,-3.5,138.291974085347));
#5663=CARTESIAN_POINT('Origin',(-2.22044604925031E-15,-3.,114.33240815703));
#5664=CARTESIAN_POINT('Origin',(-2.22044604925031E-15,-2.9,114.33240815703));
#5665=CARTESIAN_POINT('Origin',(-2.22044604925031E-15,-3.,114.33240815703));
#5666=CARTESIAN_POINT('Origin',(-2.22044604925031E-15,-2.9,114.33240815703));
#5667=CARTESIAN_POINT('Origin',(0.,-2.9,114.33240815703));
#5668=CARTESIAN_POINT('',(0.,0.,0.));
#5669=CARTESIAN_POINT('Origin',(27.848517275114,2.,0.));
#5670=CARTESIAN_POINT('',(27.848517275114,2.,133.837794222876));
#5671=CARTESIAN_POINT('',(-27.848517275114,2.,133.837794222876));
#5672=CARTESIAN_POINT('Origin',(-2.22044604925031E-15,2.,114.33240815703));
#5673=CARTESIAN_POINT('',(27.848517275114,2.,135.532881868193));
#5674=CARTESIAN_POINT('',(27.848517275114,2.,0.));
#5675=CARTESIAN_POINT('',(-27.848517275114,2.,135.532881868193));
#5676=CARTESIAN_POINT('Origin',(-2.22044604925031E-15,2.,114.33240815703));
#5677=CARTESIAN_POINT('',(-27.848517275114,2.,0.));
#5678=CARTESIAN_POINT('Origin',(-27.848517275114,2.,0.));
#5679=CARTESIAN_POINT('',(-27.848517275114,-3.,133.837794222876));
#5680=CARTESIAN_POINT('',(-27.848517275114,-4.,133.837794222876));
#5681=CARTESIAN_POINT('',(-27.848517275114,-3.,135.532881868193));
#5682=CARTESIAN_POINT('',(-27.848517275114,-4.,135.532881868193));
#5683=CARTESIAN_POINT('',(-27.848517275114,-3.,0.));
#5684=CARTESIAN_POINT('Origin',(27.848517275114,-3.,0.));
#5685=CARTESIAN_POINT('',(27.848517275114,-3.,133.837794222876));
#5686=CARTESIAN_POINT('',(27.848517275114,-4.,133.837794222876));
#5687=CARTESIAN_POINT('',(27.848517275114,-3.,135.532881868193));
#5688=CARTESIAN_POINT('',(27.848517275114,-3.,0.));
#5689=CARTESIAN_POINT('',(27.848517275114,-4.,135.532881868193));
#5690=CARTESIAN_POINT('Origin',(-2.22044604925031E-15,-4.,114.33240815703));
#5691=CARTESIAN_POINT('',(-34.,3.,114.33240815703));
#5692=CARTESIAN_POINT('Origin',(-2.22044604925031E-15,3.,114.33240815703));
#5693=CARTESIAN_POINT('',(-34.,-3.,114.33240815703));
#5694=CARTESIAN_POINT('',(-34.,-4.,114.33240815703));
#5695=CARTESIAN_POINT('Origin',(-2.22044604925031E-15,-3.,114.33240815703));
#5696=CARTESIAN_POINT('Origin',(-2.22044604925031E-15,-3.,114.33240815703));
#5697=CARTESIAN_POINT('Origin',(-2.22044604925031E-15,-4.,114.33240815703));
#5698=CARTESIAN_POINT('',(-35.,3.,114.33240815703));
#5699=CARTESIAN_POINT('Origin',(-2.22044604925031E-15,3.,114.33240815703));
#5700=CARTESIAN_POINT('',(-35.,-4.,114.33240815703));
#5701=CARTESIAN_POINT('',(-35.,-4.,114.33240815703));
#5702=CARTESIAN_POINT('Origin',(-2.22044604925031E-15,-4.,114.33240815703));
#5703=CARTESIAN_POINT('Origin',(-2.22044604925031E-15,-3.,114.33240815703));
#5704=CARTESIAN_POINT('Origin',(0.,3.,114.33240815703));
#5705=CARTESIAN_POINT('Origin',(-16.7482292407074,-4.,90.3728422287138));
#5706=CARTESIAN_POINT('',(-17.8482292407074,-3.,90.3728422287138));
#5707=CARTESIAN_POINT('Origin',(-16.7482292407074,-3.,90.3728422287138));
#5708=CARTESIAN_POINT('',(-17.8482292407074,-4.,90.3728422287138));
#5709=CARTESIAN_POINT('',(-17.8482292407074,-4.,90.3728422287138));
#5710=CARTESIAN_POINT('Origin',(-16.7482292407074,-4.,90.3728422287138));
#5711=CARTESIAN_POINT('Origin',(-6.30441727387072,-4.,85.7873857361326));
#5712=CARTESIAN_POINT('',(-7.40441727387072,-3.,85.7873857361326));
#5713=CARTESIAN_POINT('Origin',(-6.30441727387072,-3.,85.7873857361326));
#5714=CARTESIAN_POINT('',(-7.40441727387072,-4.,85.7873857361326));
#5715=CARTESIAN_POINT('',(-7.40441727387072,-4.,85.7873857361326));
#5716=CARTESIAN_POINT('Origin',(-6.30441727387072,-4.,85.7873857361326));
#5717=CARTESIAN_POINT('Origin',(-2.22044604925031E-15,-4.,114.33240815703));
#5718=CARTESIAN_POINT('',(-25.,-3.,114.33240815703));
#5719=CARTESIAN_POINT('Origin',(-2.22044604925031E-15,-3.,114.33240815703));
#5720=CARTESIAN_POINT('',(-25.,-4.,114.33240815703));
#5721=CARTESIAN_POINT('',(-25.,-4.,114.33240815703));
#5722=CARTESIAN_POINT('Origin',(-2.22044604925031E-15,-4.,114.33240815703));
#5723=CARTESIAN_POINT('Origin',(24.6422751287225,-4.,130.058890874186));
#5724=CARTESIAN_POINT('',(23.5422751287225,-3.,130.058890874186));
#5725=CARTESIAN_POINT('Origin',(24.6422751287225,-3.,130.058890874186));
#5726=CARTESIAN_POINT('',(23.5422751287225,-4.,130.058890874186));
#5727=CARTESIAN_POINT('',(23.5422751287225,-4.,130.058890874186));
#5728=CARTESIAN_POINT('Origin',(24.6422751287225,-4.,130.058890874186));
#5729=CARTESIAN_POINT('Origin',(6.30441727387071,-4.,142.877430577928));
#5730=CARTESIAN_POINT('',(5.20441727387071,-3.,142.877430577928));
#5731=CARTESIAN_POINT('Origin',(6.30441727387071,-3.,142.877430577928));
#5732=CARTESIAN_POINT('',(5.20441727387071,-4.,142.877430577928));
#5733=CARTESIAN_POINT('',(5.20441727387071,-4.,142.877430577928));
#5734=CARTESIAN_POINT('Origin',(6.30441727387071,-4.,142.877430577928));
#5735=CARTESIAN_POINT('Origin',(-15.7264827171553,-4.,138.974683285753));
#5736=CARTESIAN_POINT('',(-16.8264827171553,-3.,138.974683285753));
#5737=CARTESIAN_POINT('Origin',(-15.7264827171553,-3.,138.974683285753));
#5738=CARTESIAN_POINT('',(-16.8264827171553,-4.,138.974683285753));
#5739=CARTESIAN_POINT('',(-16.8264827171553,-4.,138.974683285753));
#5740=CARTESIAN_POINT('Origin',(-15.7264827171553,-4.,138.974683285753));
#5741=CARTESIAN_POINT('Origin',(16.7482292407074,-4.,138.291974085347));
#5742=CARTESIAN_POINT('',(15.6482292407074,-3.,138.291974085347));
#5743=CARTESIAN_POINT('Origin',(16.7482292407074,-3.,138.291974085347));
#5744=CARTESIAN_POINT('',(15.6482292407074,-4.,138.291974085347));
#5745=CARTESIAN_POINT('',(15.6482292407074,-4.,138.291974085347));
#5746=CARTESIAN_POINT('Origin',(16.7482292407074,-4.,138.291974085347));
#5747=CARTESIAN_POINT('Origin',(28.7847580111699,-4.,119.431593230258));
#5748=CARTESIAN_POINT('',(27.6847580111699,-3.,119.431593230258));
#5749=CARTESIAN_POINT('Origin',(28.7847580111699,-3.,119.431593230258));
#5750=CARTESIAN_POINT('',(27.6847580111699,-4.,119.431593230258));
#5751=CARTESIAN_POINT('',(27.6847580111699,-4.,119.431593230258));
#5752=CARTESIAN_POINT('Origin',(28.7847580111699,-4.,119.431593230258));
#5753=CARTESIAN_POINT('Origin',(-23.9595659283167,-4.,131.080637397738));
#5754=CARTESIAN_POINT('',(-25.0595659283167,-3.,131.080637397738));
#5755=CARTESIAN_POINT('Origin',(-23.9595659283167,-3.,131.080637397738));
#5756=CARTESIAN_POINT('',(-25.0595659283167,-4.,131.080637397738));
#5757=CARTESIAN_POINT('',(-25.0595659283167,-4.,131.080637397738));
#5758=CARTESIAN_POINT('Origin',(-23.9595659283167,-4.,131.080637397738));
#5759=CARTESIAN_POINT('Origin',(15.7264827171553,-4.,89.6901330283079));
#5760=CARTESIAN_POINT('',(14.6264827171553,-3.,89.6901330283079));
#5761=CARTESIAN_POINT('Origin',(15.7264827171553,-3.,89.6901330283079));
#5762=CARTESIAN_POINT('',(14.6264827171553,-4.,89.6901330283079));
#5763=CARTESIAN_POINT('',(14.6264827171553,-4.,89.6901330283079));
#5764=CARTESIAN_POINT('Origin',(15.7264827171553,-4.,89.6901330283079));
#5765=CARTESIAN_POINT('Origin',(5.09918507322788,-4.,85.5476501458605));
#5766=CARTESIAN_POINT('',(3.99918507322788,-3.,85.5476501458605));
#5767=CARTESIAN_POINT('Origin',(5.09918507322788,-3.,85.5476501458605));
#5768=CARTESIAN_POINT('',(3.99918507322788,-4.,85.5476501458605));
#5769=CARTESIAN_POINT('',(3.99918507322788,-4.,85.5476501458605));
#5770=CARTESIAN_POINT('Origin',(5.09918507322788,-4.,85.5476501458605));
#5771=CARTESIAN_POINT('Origin',(-28.5450224208979,-4.,120.636825430901));
#5772=CARTESIAN_POINT('',(-29.6450224208979,-3.,120.636825430901));
#5773=CARTESIAN_POINT('Origin',(-28.5450224208979,-3.,120.636825430901));
#5774=CARTESIAN_POINT('',(-29.6450224208979,-4.,120.636825430901));
#5775=CARTESIAN_POINT('',(-29.6450224208979,-4.,120.636825430901));
#5776=CARTESIAN_POINT('Origin',(-28.5450224208979,-4.,120.636825430901));
#5777=CARTESIAN_POINT('Origin',(-24.6422751287225,-4.,98.6059254398751));
#5778=CARTESIAN_POINT('',(-25.7422751287225,-3.,98.6059254398751));
#5779=CARTESIAN_POINT('Origin',(-24.6422751287225,-3.,98.6059254398751));
#5780=CARTESIAN_POINT('',(-25.7422751287225,-4.,98.6059254398751));
#5781=CARTESIAN_POINT('',(-25.7422751287225,-4.,98.6059254398751));
#5782=CARTESIAN_POINT('Origin',(-24.6422751287225,-4.,98.6059254398751));
#5783=CARTESIAN_POINT('Origin',(28.5450224208979,-4.,108.02799088316));
#5784=CARTESIAN_POINT('',(27.4450224208979,-3.,108.02799088316));
#5785=CARTESIAN_POINT('Origin',(28.5450224208979,-3.,108.02799088316));
#5786=CARTESIAN_POINT('',(27.4450224208979,-4.,108.02799088316));
#5787=CARTESIAN_POINT('',(27.4450224208979,-4.,108.02799088316));
#5788=CARTESIAN_POINT('Origin',(28.5450224208979,-4.,108.02799088316));
#5789=CARTESIAN_POINT('Origin',(23.9595659283167,-4.,97.584178916323));
#5790=CARTESIAN_POINT('',(22.8595659283167,-3.,97.584178916323));
#5791=CARTESIAN_POINT('Origin',(23.9595659283167,-3.,97.584178916323));
#5792=CARTESIAN_POINT('',(22.8595659283167,-4.,97.584178916323));
#5793=CARTESIAN_POINT('',(22.8595659283167,-4.,97.584178916323));
#5794=CARTESIAN_POINT('Origin',(23.9595659283167,-4.,97.584178916323));
#5795=CARTESIAN_POINT('Origin',(-28.7847580111699,-4.,109.233223083803));
#5796=CARTESIAN_POINT('',(-29.8847580111699,-3.,109.233223083803));
#5797=CARTESIAN_POINT('Origin',(-28.7847580111699,-3.,109.233223083803));
#5798=CARTESIAN_POINT('',(-29.8847580111699,-4.,109.233223083803));
#5799=CARTESIAN_POINT('',(-29.8847580111699,-4.,109.233223083803));
#5800=CARTESIAN_POINT('Origin',(-28.7847580111699,-4.,109.233223083803));
#5801=CARTESIAN_POINT('Origin',(-5.09918507322789,-4.,143.1171661682));
#5802=CARTESIAN_POINT('',(-6.19918507322789,-3.,143.1171661682));
#5803=CARTESIAN_POINT('Origin',(-5.09918507322789,-3.,143.1171661682));
#5804=CARTESIAN_POINT('',(-6.19918507322789,-4.,143.1171661682));
#5805=CARTESIAN_POINT('',(-6.19918507322789,-4.,143.1171661682));
#5806=CARTESIAN_POINT('Origin',(-5.09918507322789,-4.,143.1171661682));
#5807=CARTESIAN_POINT('Origin',(0.,-4.,114.33240815703));
#5808=CARTESIAN_POINT('Origin',(0.,-3.,114.33240815703));
#5809=CARTESIAN_POINT('',(0.,0.,0.));
#5810=CARTESIAN_POINT('Origin',(0.,-4.,114.33240815703));
#5811=CARTESIAN_POINT('',(3.14621650000503,-4.,74.4563336042978));
#5812=CARTESIAN_POINT('',(3.04264759680545,-4.,74.6493853941201));
#5813=CARTESIAN_POINT('Ctrl Pts',(3.14621650000503,-4.,74.4563336042978));
#5814=CARTESIAN_POINT('Ctrl Pts',(3.09410761398192,-4.,74.5544748329615));
#5815=CARTESIAN_POINT('Ctrl Pts',(3.04264759680544,-4.,74.6493853941201));
#5816=CARTESIAN_POINT('',(-3.14621650000503,-4.,74.4563336042978));
#5817=CARTESIAN_POINT('Origin',(0.,-4.,114.33240815703));
#5818=CARTESIAN_POINT('',(-3.04264759680545,-4.,74.6493853941201));
#5819=CARTESIAN_POINT('Ctrl Pts',(-3.04264759680544,-4.,74.6493853941201));
#5820=CARTESIAN_POINT('Ctrl Pts',(-3.09410761398192,-4.,74.5544748329615));
#5821=CARTESIAN_POINT('Ctrl Pts',(-3.14621650000503,-4.,74.4563336042978));
#5822=CARTESIAN_POINT('Origin',(-4.44089209850063E-15,-4.,114.33240815703));
#5823=CARTESIAN_POINT('Origin',(0.,0.,114.33240815703));
#5824=CARTESIAN_POINT('',(5.02570436837922,0.,74.6493853941201));
#5825=CARTESIAN_POINT('',(3.14621650000503,4.,74.4563336042978));
#5826=CARTESIAN_POINT('Ctrl Pts',(5.0257043683792,1.38777878078145E-16,
74.6493853941202));
#5827=CARTESIAN_POINT('Ctrl Pts',(5.0257043683792,0.636791095581352,74.6493853941202));
#5828=CARTESIAN_POINT('Ctrl Pts',(4.90246224678715,1.31704352377502,74.63316071429));
#5829=CARTESIAN_POINT('Ctrl Pts',(4.39842345787458,2.57251995336055,74.5741605152364));
#5830=CARTESIAN_POINT('Ctrl Pts',(4.01759790991964,3.14777098226807,74.5322097357543));
#5831=CARTESIAN_POINT('Ctrl Pts',(3.44263279831291,3.74199212690276,74.4806062316187));
#5832=CARTESIAN_POINT('Ctrl Pts',(3.29909000169272,3.87471942228721,74.4683953014136));
#5833=CARTESIAN_POINT('Ctrl Pts',(3.14621650000503,4.,74.4563336042978));
#5834=CARTESIAN_POINT('',(-3.14621650000503,4.,74.4563336042978));
#5835=CARTESIAN_POINT('Origin',(0.,4.,114.33240815703));
#5836=CARTESIAN_POINT('',(-5.02570436837922,0.,74.6493853941201));
#5837=CARTESIAN_POINT('Ctrl Pts',(-3.14621650000503,4.,74.4563336042978));
#5838=CARTESIAN_POINT('Ctrl Pts',(-3.29909000169272,3.87471942228721,74.4683953014136));
#5839=CARTESIAN_POINT('Ctrl Pts',(-3.4426327983129,3.74199212690276,74.4806062316187));
#5840=CARTESIAN_POINT('Ctrl Pts',(-4.01759790991964,3.14777098226807,74.5322097357543));
#5841=CARTESIAN_POINT('Ctrl Pts',(-4.39842345787458,2.57251995336055,74.5741605152364));
#5842=CARTESIAN_POINT('Ctrl Pts',(-4.90246224678715,1.31704352377502,74.63316071429));
#5843=CARTESIAN_POINT('Ctrl Pts',(-5.0257043683792,0.636791095581352,74.6493853941202));
#5844=CARTESIAN_POINT('Ctrl Pts',(-5.0257043683792,0.,74.6493853941202));
#5845=CARTESIAN_POINT('Ctrl Pts',(-5.0257043683792,4.16333634234434E-16,
74.6493853941202));
#5846=CARTESIAN_POINT('Ctrl Pts',(-5.0257043683792,-0.636791095581351,74.6493853941202));
#5847=CARTESIAN_POINT('Ctrl Pts',(-4.90246224678715,-1.31704352377502,74.63316071429));
#5848=CARTESIAN_POINT('Ctrl Pts',(-4.39842345787458,-2.57251995336055,74.5741605152364));
#5849=CARTESIAN_POINT('Ctrl Pts',(-4.01759790991964,-3.14777098226807,74.5322097357543));
#5850=CARTESIAN_POINT('Ctrl Pts',(-3.44263279831291,-3.74199212690276,74.4806062316187));
#5851=CARTESIAN_POINT('Ctrl Pts',(-3.29909000169272,-3.87471942228721,74.4683953014136));
#5852=CARTESIAN_POINT('Ctrl Pts',(-3.14621650000503,-4.,74.4563336042978));
#5853=CARTESIAN_POINT('Ctrl Pts',(3.14621650000503,-4.,74.4563336042978));
#5854=CARTESIAN_POINT('Ctrl Pts',(3.29909000173959,-3.8747194222488,74.4683953014173));
#5855=CARTESIAN_POINT('Ctrl Pts',(3.44263279838552,-3.74199212682772,74.4806062316253));
#5856=CARTESIAN_POINT('Ctrl Pts',(4.01759790991964,-3.14777098226807,74.5322097357543));
#5857=CARTESIAN_POINT('Ctrl Pts',(4.39842345787458,-2.57251995336055,74.5741605152364));
#5858=CARTESIAN_POINT('Ctrl Pts',(4.90246224678715,-1.31704352377502,74.63316071429));
#5859=CARTESIAN_POINT('Ctrl Pts',(5.0257043683792,-0.636791095581352,74.6493853941202));
#5860=CARTESIAN_POINT('Ctrl Pts',(5.0257043683792,-4.16333634234434E-16,
74.6493853941202));
#5861=CARTESIAN_POINT('Origin',(0.,4.,114.33240815703));
#5862=CARTESIAN_POINT('',(3.04264759680545,4.,74.6493853941201));
#5863=CARTESIAN_POINT('Ctrl Pts',(3.04264759680544,4.,74.6493853941201));
#5864=CARTESIAN_POINT('Ctrl Pts',(3.09410761398192,4.,74.5544748329615));
#5865=CARTESIAN_POINT('Ctrl Pts',(3.14621650000503,4.,74.4563336042978));
#5866=CARTESIAN_POINT('',(-3.04264759680545,4.,74.6493853941201));
#5867=CARTESIAN_POINT('Origin',(-4.44089209850063E-15,4.,114.33240815703));
#5868=CARTESIAN_POINT('Ctrl Pts',(-3.14621650000503,4.,74.4563336042978));
#5869=CARTESIAN_POINT('Ctrl Pts',(-3.09410761398192,4.,74.5544748329615));
#5870=CARTESIAN_POINT('Ctrl Pts',(-3.04264759680544,4.,74.6493853941201));
#5871=CARTESIAN_POINT('Origin',(-4.44089209850063E-15,0.,114.33240815703));
#5872=CARTESIAN_POINT('Origin',(0.,0.,74.6493853941201));
#5873=CARTESIAN_POINT('Origin',(-4.44089209850063E-15,0.,114.33240815703));
#5874=CARTESIAN_POINT('Origin',(0.,0.,74.6493853941201));
#5875=CARTESIAN_POINT('Origin',(0.,0.,0.5));
#5876=CARTESIAN_POINT('',(-5.,-6.12323399573677E-16,0.));
#5877=CARTESIAN_POINT('Origin',(0.,0.,0.));
#5878=CARTESIAN_POINT('',(-6.,7.34788079488412E-16,1.));
#5879=CARTESIAN_POINT('',(-5.5,6.73555739531044E-16,0.5));
#5880=CARTESIAN_POINT('',(6.,-7.34788079488412E-16,1.));
#5881=CARTESIAN_POINT('Origin',(0.,0.,1.));
#5882=CARTESIAN_POINT('Origin',(0.,0.,1.));
#5883=CARTESIAN_POINT('Origin',(0.,0.,35.8406354386459));
#5884=CARTESIAN_POINT('',(6.,-7.34788079488412E-16,71.6812708772919));
#5885=CARTESIAN_POINT('',(6.,-7.34788079488412E-16,35.8406354386459));
#5886=CARTESIAN_POINT('Origin',(0.,0.,71.6812708772919));
#5887=CARTESIAN_POINT('Origin',(0.,0.,0.));
#5888=CARTESIAN_POINT('Origin',(0.,0.,73.165328135706));
#5889=CARTESIAN_POINT('',(5.51285218418961,-6.7512967815403E-16,73.165328135706));
#5890=CARTESIAN_POINT('',(0.,0.,0.));
#5891=CARTESIAN_POINT('Origin',(-2.77555756156289E-16,0.75,150.));
#5892=CARTESIAN_POINT('',(-0.75,0.75,148.324135091683));
#5893=CARTESIAN_POINT('Ctrl Pts',(-0.75,0.75,148.324135091683));
#5894=CARTESIAN_POINT('Ctrl Pts',(-0.75,0.844174950069239,148.324135091683));
#5895=CARTESIAN_POINT('Ctrl Pts',(-0.731178490330683,0.944625017929177,
148.324566712535));
#5896=CARTESIAN_POINT('Ctrl Pts',(-0.654637296400931,1.12940860934839,148.326126918842));
#5897=CARTESIAN_POINT('Ctrl Pts',(-0.596917780711965,1.21374239106786,148.327233118533));
#5898=CARTESIAN_POINT('Ctrl Pts',(-0.463742391599736,1.34691778018009,148.329310633496));
#5899=CARTESIAN_POINT('Ctrl Pts',(-0.379408609590679,1.40463729616334,148.330416715758));
#5900=CARTESIAN_POINT('Ctrl Pts',(-0.194625017492537,1.48117849064877,148.331976653629));
#5901=CARTESIAN_POINT('Ctrl Pts',(-0.0941749493170033,1.5,148.33240815703));
#5902=CARTESIAN_POINT('Ctrl Pts',(0.0941749493170025,1.5,148.33240815703));
#5903=CARTESIAN_POINT('Ctrl Pts',(0.194625017492536,1.48117849064877,148.331976653629));
#5904=CARTESIAN_POINT('Ctrl Pts',(0.379408609590678,1.40463729616334,148.330416715758));
#5905=CARTESIAN_POINT('Ctrl Pts',(0.463742391599735,1.34691778018009,148.329310633496));
#5906=CARTESIAN_POINT('Ctrl Pts',(0.596917780711964,1.21374239106786,148.327233118533));
#5907=CARTESIAN_POINT('Ctrl Pts',(0.65463729640093,1.12940860934839,148.326126918842));
#5908=CARTESIAN_POINT('Ctrl Pts',(0.731178490330683,0.944625017929177,148.324566712535));
#5909=CARTESIAN_POINT('Ctrl Pts',(0.75,0.844174950069239,148.324135091683));
#5910=CARTESIAN_POINT('Ctrl Pts',(0.75,0.655825049930761,148.324135091683));
#5911=CARTESIAN_POINT('Ctrl Pts',(0.731178490330683,0.555374982070823,148.324566712535));
#5912=CARTESIAN_POINT('Ctrl Pts',(0.65463729640093,0.370591390651611,148.326126918842));
#5913=CARTESIAN_POINT('Ctrl Pts',(0.596917780711965,0.286257608932143,148.327233118533));
#5914=CARTESIAN_POINT('Ctrl Pts',(0.463742391599736,0.153082219819914,148.329310633496));
#5915=CARTESIAN_POINT('Ctrl Pts',(0.379408609590678,0.0953627038366558,
148.330416715758));
#5916=CARTESIAN_POINT('Ctrl Pts',(0.194625017492536,0.0188215093512261,
148.331976653629));
#5917=CARTESIAN_POINT('Ctrl Pts',(0.0941749493170028,-2.48722993596056E-16,
148.33240815703));
#5918=CARTESIAN_POINT('Ctrl Pts',(-0.0941749493170028,-3.06388518716522E-16,
148.33240815703));
#5919=CARTESIAN_POINT('Ctrl Pts',(-0.194625017492536,0.0188215093512259,
148.331976653629));
#5920=CARTESIAN_POINT('Ctrl Pts',(-0.379408609590678,0.0953627038366554,
148.330416715758));
#5921=CARTESIAN_POINT('Ctrl Pts',(-0.463742391599735,0.153082219819914,
148.329310633496));
#5922=CARTESIAN_POINT('Ctrl Pts',(-0.596917780711965,0.286257608932143,
148.327233118533));
#5923=CARTESIAN_POINT('Ctrl Pts',(-0.65463729640093,0.370591390651611,148.326126918842));
#5924=CARTESIAN_POINT('Ctrl Pts',(-0.731178490330683,0.555374982070822,
148.324566712535));
#5925=CARTESIAN_POINT('Ctrl Pts',(-0.75,0.655825049930761,148.324135091683));
#5926=CARTESIAN_POINT('Ctrl Pts',(-0.75,0.75,148.324135091683));
#5927=CARTESIAN_POINT('',(-0.75,0.75,143.));
#5928=CARTESIAN_POINT('',(-0.75,0.75,150.));
#5929=CARTESIAN_POINT('Origin',(-2.77555756156289E-16,0.75,143.));
#5930=CARTESIAN_POINT('Origin',(-2.77555756156289E-16,0.75,143.));
#5931=CARTESIAN_POINT('Origin',(21.3786362834003,0.,183.365153071209));
#5932=CARTESIAN_POINT('',(6.7681855290754,-0.5,138.398809313913));
#5933=CARTESIAN_POINT('',(6.76818552907538,-2.,138.398809313913));
#5934=CARTESIAN_POINT('',(6.76818552907538,-2.,138.398809313913));
#5935=CARTESIAN_POINT('',(9.55097594168496,-0.5,146.963357554211));
#5936=CARTESIAN_POINT('',(14.9826398548955,-0.5,163.680300159368));
#5937=CARTESIAN_POINT('',(9.55097594168495,-2.,146.963357554211));
#5938=CARTESIAN_POINT('',(9.55097594168495,-2.,146.963357554211));
#5939=CARTESIAN_POINT('',(10.2137898835526,-2.,149.003289111307));
#5940=CARTESIAN_POINT('Origin',(-10.3247007219358,0.,116.635644555059));
#5941=CARTESIAN_POINT('',(-24.0664011568829,-0.5,121.100593686106));
#5942=CARTESIAN_POINT('',(-24.0664011568829,-2.,121.100593686106));
#5943=CARTESIAN_POINT('',(-24.0664011568829,-2.,121.100593686106));
#5944=CARTESIAN_POINT('',(-32.6309493971805,-0.5,123.883384098715));
#5945=CARTESIAN_POINT('',(9.36015218990532,-0.5,110.239648126554));
#5946=CARTESIAN_POINT('',(-32.6309493971805,-2.,123.883384098715));
#5947=CARTESIAN_POINT('',(-32.6309493971805,-2.,123.883384098715));
#5948=CARTESIAN_POINT('',(-5.31685885815536,-2.,115.008498097897));
#5949=CARTESIAN_POINT('Origin',(-9.10763471134047,0.,119.713424126857));
#5950=CARTESIAN_POINT('',(-20.7970232944598,-0.5,128.206262058874));
#5951=CARTESIAN_POINT('',(-20.7970232944598,-2.,128.206262058874));
#5952=CARTESIAN_POINT('',(-20.7970232944598,-2.,128.206262058874));
#5953=CARTESIAN_POINT('',(-28.082463178239,-0.5,133.499443969666));
#5954=CARTESIAN_POINT('',(7.63730133040817,-0.5,107.547515963797));
#5955=CARTESIAN_POINT('',(-28.082463178239,-2.,133.499443969666));
#5956=CARTESIAN_POINT('',(-28.082463178239,-2.,133.499443969666));
#5957=CARTESIAN_POINT('',(-4.84770998181646,-2.,116.618407644756));
#5958=CARTESIAN_POINT('Origin',(-6.99904995857679,0.,122.264472363786));
#5959=CARTESIAN_POINT('',(-15.4918878905933,-0.5,133.953860946905));
#5960=CARTESIAN_POINT('',(-15.4918878905933,-2.,133.953860946905));
#5961=CARTESIAN_POINT('',(-15.4918878905933,-2.,133.953860946905));
#5962=CARTESIAN_POINT('',(-20.7850698013853,-0.5,141.239300830684));
#5963=CARTESIAN_POINT('',(5.16685820448335,-0.5,105.519536322037));
#5964=CARTESIAN_POINT('',(-20.7850698013853,-2.,141.239300830684));
#5965=CARTESIAN_POINT('',(-20.7850698013853,-2.,141.239300830684));
#5966=CARTESIAN_POINT('',(-3.90403347647587,-2.,118.004547634262));
#5967=CARTESIAN_POINT('Origin',(-4.20534943061909,0.,124.039074890216));
#5968=CARTESIAN_POINT('',(-8.6702985616657,-0.5,137.780775325163));
#5969=CARTESIAN_POINT('',(-8.6702985616657,-2.,137.780775325163));
#5970=CARTESIAN_POINT('',(-8.6702985616657,-2.,137.780775325163));
#5971=CARTESIAN_POINT('',(-11.4530889742753,-0.5,146.345323565461));
#5972=CARTESIAN_POINT('',(2.19064699788576,-0.5,104.354221978375));
#5973=CARTESIAN_POINT('',(-11.4530889742753,-2.,146.345323565461));
#5974=CARTESIAN_POINT('',(-11.4530889742753,-2.,146.345323565461));
#5975=CARTESIAN_POINT('',(-2.57820297345712,-2.,119.031233026436));
#5976=CARTESIAN_POINT('Origin',(-0.999999999999996,0.,186.592811973533));
#5977=CARTESIAN_POINT('',(-0.999999999999999,-0.5,139.312400150624));
#5978=CARTESIAN_POINT('',(-1.,-2.,139.312400150624));
#5979=CARTESIAN_POINT('',(-1.,-2.,139.312400150624));
#5980=CARTESIAN_POINT('',(-0.999999999999998,-0.5,148.317699092963));
#5981=CARTESIAN_POINT('',(-0.999999999999996,-0.5,165.894932747045));
#5982=CARTESIAN_POINT('',(-1.,-2.,148.317699092963));
#5983=CARTESIAN_POINT('',(-1.,-2.,148.317699092963));
#5984=CARTESIAN_POINT('',(-1.,-2.,150.462610065282));
#5985=CARTESIAN_POINT('Origin',(41.6645826936637,0.,173.380088117269));
#5986=CARTESIAN_POINT('',(13.8738539018434,-0.5,135.12943145149));
#5987=CARTESIAN_POINT('',(13.8738539018434,-2.,135.12943145149));
#5988=CARTESIAN_POINT('',(13.8738539018434,-2.,135.12943145149));
#5989=CARTESIAN_POINT('',(19.1670358126354,-0.5,142.414871335269));
#5990=CARTESIAN_POINT('',(29.4986745306036,-0.5,156.635152075521));
#5991=CARTESIAN_POINT('',(19.1670358126354,-2.,142.414871335269));
#5992=CARTESIAN_POINT('',(19.1670358126354,-2.,142.414871335269));
#5993=CARTESIAN_POINT('',(20.4277828496444,-2.,144.150140763296));
#5994=CARTESIAN_POINT('Origin',(57.872109455654,0.,157.615024839444));
#5995=CARTESIAN_POINT('',(19.6214527898748,-0.5,129.824296047624));
#5996=CARTESIAN_POINT('',(19.6214527898749,-2.,129.824296047624));
#5997=CARTESIAN_POINT('',(19.6214527898749,-2.,129.824296047624));
#5998=CARTESIAN_POINT('',(26.906892673654,-0.5,135.117477958416));
#5999=CARTESIAN_POINT('',(41.1271734139054,-0.5,145.449116676384));
#6000=CARTESIAN_POINT('',(26.906892673654,-2.,135.117477958416));
#6001=CARTESIAN_POINT('',(26.906892673654,-2.,135.117477958416));
#6002=CARTESIAN_POINT('',(28.6421621016808,-2.,136.378224995425));
#6003=CARTESIAN_POINT('Origin',(68.4147109254286,0.,137.613157473021));
#6004=CARTESIAN_POINT('',(23.448367168133,-0.5,123.002706718696));
#6005=CARTESIAN_POINT('',(23.448367168133,-2.,123.002706718696));
#6006=CARTESIAN_POINT('',(23.448367168133,-2.,123.002706718696));
#6007=CARTESIAN_POINT('',(32.0129154084306,-0.5,125.785497131306));
#6008=CARTESIAN_POINT('',(48.7298580135875,-0.5,131.217161044516));
#6009=CARTESIAN_POINT('',(32.0129154084306,-2.,125.785497131306));
#6010=CARTESIAN_POINT('',(32.0129154084306,-2.,125.785497131306));
#6011=CARTESIAN_POINT('',(34.0528469655268,-2.,126.448311073173));
#6012=CARTESIAN_POINT('Origin',(72.2604038165021,0.,115.33240815703));
#6013=CARTESIAN_POINT('',(24.9799919935936,-0.5,115.33240815703));
#6014=CARTESIAN_POINT('',(24.9799919935936,-2.,115.33240815703));
#6015=CARTESIAN_POINT('',(24.9799919935936,-2.,115.33240815703));
#6016=CARTESIAN_POINT('',(33.9852909359328,-0.5,115.33240815703));
#6017=CARTESIAN_POINT('',(51.5625245900145,-0.5,115.33240815703));
#6018=CARTESIAN_POINT('',(33.9852909359328,-2.,115.33240815703));
#6019=CARTESIAN_POINT('',(33.9852909359328,-2.,115.33240815703));
#6020=CARTESIAN_POINT('',(36.1302019082511,-2.,115.33240815703));
#6021=CARTESIAN_POINT('Origin',(69.0327449141785,0.,92.9537718736301));
#6022=CARTESIAN_POINT('',(24.0664011568829,-0.5,107.564222627955));
#6023=CARTESIAN_POINT('',(24.0664011568829,-2.,107.564222627955));
#6024=CARTESIAN_POINT('',(24.0664011568829,-2.,107.564222627955));
#6025=CARTESIAN_POINT('',(32.6309493971805,-0.5,104.781432215346));
#6026=CARTESIAN_POINT('',(49.3478920023374,-0.5,99.349768302135));
#6027=CARTESIAN_POINT('',(32.6309493971805,-2.,104.781432215346));
#6028=CARTESIAN_POINT('',(32.6309493971805,-2.,104.781432215346));
#6029=CARTESIAN_POINT('',(34.6708809542767,-2.,104.118618273478));
#6030=CARTESIAN_POINT('Origin',(59.047679960239,0.,72.6678254633667));
#6031=CARTESIAN_POINT('',(20.7970232944598,-0.5,100.458554255187));
#6032=CARTESIAN_POINT('',(20.7970232944598,-2.,100.458554255187));
#6033=CARTESIAN_POINT('',(20.7970232944598,-2.,100.458554255187));
#6034=CARTESIAN_POINT('',(28.082463178239,-0.5,95.165372344395));
#6035=CARTESIAN_POINT('',(42.3027439184904,-0.5,84.8337336264269));
#6036=CARTESIAN_POINT('',(28.082463178239,-2.,95.165372344395));
#6037=CARTESIAN_POINT('',(28.082463178239,-2.,95.165372344395));
#6038=CARTESIAN_POINT('',(29.8177326062657,-2.,93.9046253073861));
#6039=CARTESIAN_POINT('Origin',(43.2826166824136,0.,56.4602987013764));
#6040=CARTESIAN_POINT('',(15.4918878905933,-0.5,94.7109553671556));
#6041=CARTESIAN_POINT('',(15.4918878905933,-2.,94.7109553671556));
#6042=CARTESIAN_POINT('',(15.4918878905933,-2.,94.7109553671556));
#6043=CARTESIAN_POINT('',(20.7850698013853,-0.5,87.4255154833764));
#6044=CARTESIAN_POINT('',(31.1167085193535,-0.5,73.205234743125));
#6045=CARTESIAN_POINT('',(20.7850698013853,-2.,87.4255154833764));
#6046=CARTESIAN_POINT('',(20.7850698013853,-2.,87.4255154833764));
#6047=CARTESIAN_POINT('',(22.0458168383943,-2.,85.6902460553496));
#6048=CARTESIAN_POINT('Origin',(23.2807493159906,0.,45.9176972316019));
#6049=CARTESIAN_POINT('',(8.6702985616657,-0.5,90.8840409888974));
#6050=CARTESIAN_POINT('',(8.6702985616657,-2.,90.8840409888975));
#6051=CARTESIAN_POINT('',(8.6702985616657,-2.,90.8840409888975));
#6052=CARTESIAN_POINT('',(11.4530889742753,-0.5,82.3194927485999));
#6053=CARTESIAN_POINT('',(16.8847528874858,-0.5,65.602550143443));
#6054=CARTESIAN_POINT('',(11.4530889742753,-2.,82.3194927485999));
#6055=CARTESIAN_POINT('',(11.4530889742753,-2.,82.3194927485999));
#6056=CARTESIAN_POINT('',(12.1159029161429,-2.,80.2795611915036));
#6057=CARTESIAN_POINT('Origin',(-2.30323639802878,0.,104.007707435095));
#6058=CARTESIAN_POINT('',(-6.76818552907538,-0.5,90.2660070001475));
#6059=CARTESIAN_POINT('',(-6.76818552907539,-2.,90.2660070001475));
#6060=CARTESIAN_POINT('',(-6.76818552907539,-2.,90.2660070001475));
#6061=CARTESIAN_POINT('',(-9.55097594168494,-0.5,81.70145875985));
#6062=CARTESIAN_POINT('',(4.09276003047609,-0.5,123.692560346936));
#6063=CARTESIAN_POINT('',(-9.55097594168495,-2.,81.70145875985));
#6064=CARTESIAN_POINT('',(-9.55097594168495,-2.,81.70145875985));
#6065=CARTESIAN_POINT('',(-0.67608994086681,-2.,109.015549298875));
#6066=CARTESIAN_POINT('Origin',(-5.38101596982691,0.,105.22477344569));
#6067=CARTESIAN_POINT('',(-13.8738539018434,-0.5,93.5353848625706));
#6068=CARTESIAN_POINT('',(-13.8738539018435,-2.,93.5353848625707));
#6069=CARTESIAN_POINT('',(-13.8738539018435,-2.,93.5353848625707));
#6070=CARTESIAN_POINT('',(-19.1670358126355,-0.5,86.2499449787914));
#6071=CARTESIAN_POINT('',(6.78489219323324,-0.5,121.969709487439));
#6072=CARTESIAN_POINT('',(-19.1670358126355,-2.,86.2499449787915));
#6073=CARTESIAN_POINT('',(-19.1670358126355,-2.,86.2499449787915));
#6074=CARTESIAN_POINT('',(-2.285999487726,-2.,109.484698175214));
#6075=CARTESIAN_POINT('Origin',(-7.93206420675555,0.,107.333358198454));
#6076=CARTESIAN_POINT('',(-19.6214527898749,-0.5,98.8405202664372));
#6077=CARTESIAN_POINT('',(-19.6214527898749,-2.,98.8405202664371));
#6078=CARTESIAN_POINT('',(-19.6214527898749,-2.,98.8405202664371));
#6079=CARTESIAN_POINT('',(-26.9068926736541,-0.5,93.5473383556452));
#6080=CARTESIAN_POINT('',(8.81287183499309,-0.5,119.499266361514));
#6081=CARTESIAN_POINT('',(-26.9068926736541,-2.,93.5473383556451));
#6082=CARTESIAN_POINT('',(-26.9068926736541,-2.,93.5473383556451));
#6083=CARTESIAN_POINT('',(-3.67213947723154,-2.,110.428374680555));
#6084=CARTESIAN_POINT('Origin',(-9.70666673318587,0.,110.127058726411));
#6085=CARTESIAN_POINT('',(-23.448367168133,-0.5,105.662109595365));
#6086=CARTESIAN_POINT('',(-23.448367168133,-2.,105.662109595365));
#6087=CARTESIAN_POINT('',(-23.448367168133,-2.,105.662109595365));
#6088=CARTESIAN_POINT('',(-32.0129154084306,-0.5,102.879319182755));
#6089=CARTESIAN_POINT('',(9.97818617865523,-0.5,116.523055154916));
#6090=CARTESIAN_POINT('',(-32.0129154084306,-2.,102.879319182755));
#6091=CARTESIAN_POINT('',(-32.0129154084306,-2.,102.879319182755));
#6092=CARTESIAN_POINT('',(-4.69882486940547,-2.,111.754205183573));
#6093=CARTESIAN_POINT('Origin',(-10.5311130894481,0.,113.33240815703));
#6094=CARTESIAN_POINT('',(-24.9799919935936,-0.5,113.33240815703));
#6095=CARTESIAN_POINT('',(-24.9799919935936,-2.,113.33240815703));
#6096=CARTESIAN_POINT('',(-24.9799919935936,-2.,113.33240815703));
#6097=CARTESIAN_POINT('',(-33.9852909359328,-0.5,113.33240815703));
#6098=CARTESIAN_POINT('',(10.1667661370394,-0.5,113.33240815703));
#6099=CARTESIAN_POINT('',(-33.9852909359328,-2.,113.33240815703));
#6100=CARTESIAN_POINT('',(-33.9852909359328,-2.,113.33240815703));
#6101=CARTESIAN_POINT('',(-5.26555654472407,-2.,113.33240815703));
#6102=CARTESIAN_POINT('Origin',(9.53769994268576,-0.5,84.9783860609091));
#6103=CARTESIAN_POINT('',(-24.9799919935936,-0.5,115.33240815703));
#6104=CARTESIAN_POINT('',(-25.,-0.5,114.33240815703));
#6105=CARTESIAN_POINT('Origin',(-2.22044604925031E-15,-0.5,114.33240815703));
#6106=CARTESIAN_POINT('',(-33.9852909359328,-0.5,115.33240815703));
#6107=CARTESIAN_POINT('',(-10.1667661370394,-0.5,115.33240815703));
#6108=CARTESIAN_POINT('',(-34.,-0.5,114.33240815703));
#6109=CARTESIAN_POINT('Origin',(-2.22044604925031E-15,-0.5,114.33240815703));
#6110=CARTESIAN_POINT('Origin',(-2.22044604925031E-15,-0.5,114.33240815703));
#6111=CARTESIAN_POINT('Origin',(-2.22044604925031E-15,-0.5,114.33240815703));
#6112=CARTESIAN_POINT('Origin',(9.53769994268576,-0.5,84.9783860609091));
#6113=CARTESIAN_POINT('',(-24.0664011568829,-0.5,107.564222627955));
#6114=CARTESIAN_POINT('Origin',(-2.22044604925031E-15,-0.5,114.33240815703));
#6115=CARTESIAN_POINT('',(-32.6309493971805,-0.5,104.781432215346));
#6116=CARTESIAN_POINT('',(-9.97818617865522,-0.5,112.141761159145));
#6117=CARTESIAN_POINT('Origin',(-2.22044604925031E-15,-0.5,114.33240815703));
#6118=CARTESIAN_POINT('Origin',(9.53769994268576,-0.5,84.9783860609091));
#6119=CARTESIAN_POINT('',(-20.7970232944598,-0.5,100.458554255187));
#6120=CARTESIAN_POINT('Origin',(-2.22044604925031E-15,-0.5,114.33240815703));
#6121=CARTESIAN_POINT('',(-28.082463178239,-0.5,95.165372344395));
#6122=CARTESIAN_POINT('',(-8.81287183499312,-0.5,109.165549952547));
#6123=CARTESIAN_POINT('Origin',(-2.22044604925031E-15,-0.5,114.33240815703));
#6124=CARTESIAN_POINT('Origin',(9.53769994268576,-0.5,84.9783860609091));
#6125=CARTESIAN_POINT('',(-15.4918878905933,-0.5,94.7109553671556));
#6126=CARTESIAN_POINT('Origin',(-2.22044604925031E-15,-0.5,114.33240815703));
#6127=CARTESIAN_POINT('',(-20.7850698013853,-0.5,87.4255154833764));
#6128=CARTESIAN_POINT('',(-6.78489219323324,-0.5,106.695106826622));
#6129=CARTESIAN_POINT('Origin',(-2.22044604925031E-15,-0.5,114.33240815703));
#6130=CARTESIAN_POINT('Origin',(9.53769994268576,-0.5,84.9783860609091));
#6131=CARTESIAN_POINT('',(-8.67029856166571,-0.5,90.8840409888974));
#6132=CARTESIAN_POINT('Origin',(-2.22044604925031E-15,-0.5,114.33240815703));
#6133=CARTESIAN_POINT('',(-11.4530889742753,-0.5,82.3194927485999));
#6134=CARTESIAN_POINT('',(-4.09276003047608,-0.5,104.972255967125));
#6135=CARTESIAN_POINT('Origin',(-2.22044604925031E-15,-0.5,114.33240815703));
#6136=CARTESIAN_POINT('Origin',(9.53769994268576,-0.5,84.9783860609091));
#6137=CARTESIAN_POINT('',(6.76818552907538,-0.5,90.2660070001475));
#6138=CARTESIAN_POINT('Origin',(-2.22044604925031E-15,-0.5,114.33240815703));
#6139=CARTESIAN_POINT('',(9.55097594168495,-0.5,81.70145875985));
#6140=CARTESIAN_POINT('',(2.19064699788576,-0.5,104.354221978375));
#6141=CARTESIAN_POINT('Origin',(-2.22044604925031E-15,-0.5,114.33240815703));
#6142=CARTESIAN_POINT('Origin',(9.53769994268576,-0.5,84.9783860609091));
#6143=CARTESIAN_POINT('',(13.8738539018434,-0.5,93.5353848625706));
#6144=CARTESIAN_POINT('Origin',(-2.22044604925031E-15,-0.5,114.33240815703));
#6145=CARTESIAN_POINT('',(19.1670358126354,-0.5,86.2499449787914));
#6146=CARTESIAN_POINT('',(5.16685820448335,-0.5,105.519536322037));
#6147=CARTESIAN_POINT('Origin',(-2.22044604925031E-15,-0.5,114.33240815703));
#6148=CARTESIAN_POINT('Origin',(9.53769994268576,-0.5,84.9783860609091));
#6149=CARTESIAN_POINT('',(19.6214527898749,-0.5,98.8405202664372));
#6150=CARTESIAN_POINT('Origin',(-2.22044604925031E-15,-0.5,114.33240815703));
#6151=CARTESIAN_POINT('',(26.9068926736541,-0.5,93.5473383556452));
#6152=CARTESIAN_POINT('',(7.63730133040817,-0.5,107.547515963797));
#6153=CARTESIAN_POINT('Origin',(-2.22044604925031E-15,-0.5,114.33240815703));
#6154=CARTESIAN_POINT('Origin',(9.53769994268576,-0.5,84.9783860609091));
#6155=CARTESIAN_POINT('',(23.448367168133,-0.5,105.662109595365));
#6156=CARTESIAN_POINT('Origin',(-2.22044604925031E-15,-0.5,114.33240815703));
#6157=CARTESIAN_POINT('',(32.0129154084306,-0.5,102.879319182755));
#6158=CARTESIAN_POINT('',(9.36015218990532,-0.5,110.239648126554));
#6159=CARTESIAN_POINT('Origin',(-2.22044604925031E-15,-0.5,114.33240815703));
#6160=CARTESIAN_POINT('Origin',(9.53769994268576,-0.5,84.9783860609091));
#6161=CARTESIAN_POINT('',(24.9799919935936,-0.5,113.33240815703));
#6162=CARTESIAN_POINT('Origin',(-2.22044604925031E-15,-0.5,114.33240815703));
#6163=CARTESIAN_POINT('',(33.9852909359328,-0.5,113.33240815703));
#6164=CARTESIAN_POINT('',(10.1667661370394,-0.5,113.33240815703));
#6165=CARTESIAN_POINT('Origin',(-2.22044604925031E-15,-0.5,114.33240815703));
#6166=CARTESIAN_POINT('Origin',(9.53769994268576,-0.5,84.9783860609091));
#6167=CARTESIAN_POINT('',(24.0664011568829,-0.5,121.100593686106));
#6168=CARTESIAN_POINT('Origin',(-2.22044604925031E-15,-0.5,114.33240815703));
#6169=CARTESIAN_POINT('',(32.6309493971805,-0.5,123.883384098715));
#6170=CARTESIAN_POINT('',(9.97818617865523,-0.5,116.523055154916));
#6171=CARTESIAN_POINT('Origin',(-2.22044604925031E-15,-0.5,114.33240815703));
#6172=CARTESIAN_POINT('Origin',(9.53769994268576,-0.5,84.9783860609091));
#6173=CARTESIAN_POINT('',(20.7970232944598,-0.5,128.206262058874));
#6174=CARTESIAN_POINT('Origin',(-2.22044604925031E-15,-0.5,114.33240815703));
#6175=CARTESIAN_POINT('',(28.082463178239,-0.5,133.499443969666));
#6176=CARTESIAN_POINT('',(8.81287183499309,-0.5,119.499266361514));
#6177=CARTESIAN_POINT('Origin',(-2.22044604925031E-15,-0.5,114.33240815703));
#6178=CARTESIAN_POINT('Origin',(9.53769994268576,-0.5,84.9783860609091));
#6179=CARTESIAN_POINT('',(15.4918878905933,-0.5,133.953860946905));
#6180=CARTESIAN_POINT('Origin',(-2.22044604925031E-15,-0.5,114.33240815703));
#6181=CARTESIAN_POINT('',(20.7850698013853,-0.5,141.239300830684));
#6182=CARTESIAN_POINT('',(6.78489219323324,-0.5,121.969709487439));
#6183=CARTESIAN_POINT('Origin',(-2.22044604925031E-15,-0.5,114.33240815703));
#6184=CARTESIAN_POINT('Origin',(9.53769994268576,-0.5,84.9783860609091));
#6185=CARTESIAN_POINT('',(1.,-0.5,139.312400150624));
#6186=CARTESIAN_POINT('Origin',(-2.22044604925031E-15,-0.5,114.33240815703));
#6187=CARTESIAN_POINT('',(1.,-0.5,148.317699092963));
#6188=CARTESIAN_POINT('',(1.,-0.5,124.49917429407));
#6189=CARTESIAN_POINT('Origin',(-2.22044604925031E-15,-0.5,114.33240815703));
#6190=CARTESIAN_POINT('Origin',(9.53769994268576,-0.5,84.9783860609091));
#6191=CARTESIAN_POINT('',(-6.76818552907539,-0.5,138.398809313913));
#6192=CARTESIAN_POINT('Origin',(-2.22044604925031E-15,-0.5,114.33240815703));
#6193=CARTESIAN_POINT('',(-9.55097594168495,-0.5,146.963357554211));
#6194=CARTESIAN_POINT('',(-2.19064699788578,-0.5,124.310594335686));
#6195=CARTESIAN_POINT('Origin',(-2.22044604925031E-15,-0.5,114.33240815703));
#6196=CARTESIAN_POINT('Origin',(9.53769994268576,-0.5,84.9783860609091));
#6197=CARTESIAN_POINT('',(-13.8738539018434,-0.5,135.12943145149));
#6198=CARTESIAN_POINT('Origin',(-2.22044604925031E-15,-0.5,114.33240815703));
#6199=CARTESIAN_POINT('',(-19.1670358126354,-0.5,142.414871335269));
#6200=CARTESIAN_POINT('',(-5.16685820448335,-0.5,123.145279992024));
#6201=CARTESIAN_POINT('Origin',(-2.22044604925031E-15,-0.5,114.33240815703));
#6202=CARTESIAN_POINT('Origin',(9.53769994268576,-0.5,84.9783860609091));
#6203=CARTESIAN_POINT('',(-19.6214527898749,-0.5,129.824296047624));
#6204=CARTESIAN_POINT('Origin',(-2.22044604925031E-15,-0.5,114.33240815703));
#6205=CARTESIAN_POINT('',(-26.906892673654,-0.5,135.117477958416));
#6206=CARTESIAN_POINT('',(-7.63730133040816,-0.5,121.117300350264));
#6207=CARTESIAN_POINT('Origin',(-2.22044604925031E-15,-0.5,114.33240815703));
#6208=CARTESIAN_POINT('Origin',(9.53769994268576,-0.5,84.9783860609091));
#6209=CARTESIAN_POINT('',(-23.448367168133,-0.5,123.002706718696));
#6210=CARTESIAN_POINT('Origin',(-2.22044604925031E-15,-0.5,114.33240815703));
#6211=CARTESIAN_POINT('',(-32.0129154084306,-0.5,125.785497131306));
#6212=CARTESIAN_POINT('',(-9.36015218990532,-0.5,118.425168187507));
#6213=CARTESIAN_POINT('Origin',(-2.22044604925031E-15,-0.5,114.33240815703));
#6214=CARTESIAN_POINT('Origin',(9.53769994268576,-0.5,84.9783860609091));
#6215=CARTESIAN_POINT('',(8.67029856166571,-0.5,137.780775325163));
#6216=CARTESIAN_POINT('Origin',(-2.22044604925031E-15,-0.5,114.33240815703));
#6217=CARTESIAN_POINT('',(11.4530889742753,-0.5,146.345323565461));
#6218=CARTESIAN_POINT('',(4.09276003047609,-0.5,123.692560346936));
#6219=CARTESIAN_POINT('Origin',(-2.22044604925031E-15,-0.5,114.33240815703));
#6220=CARTESIAN_POINT('Origin',(-4.20534943061909,0.,124.039074890216));
#6221=CARTESIAN_POINT('',(6.76818552907538,-2.,90.2660070001475));
#6222=CARTESIAN_POINT('',(6.76818552907538,-2.,90.2660070001475));
#6223=CARTESIAN_POINT('',(9.55097594168495,-2.,81.70145875985));
#6224=CARTESIAN_POINT('',(-2.57820297345712,-2.,119.031233026436));
#6225=CARTESIAN_POINT('',(9.55097594168495,-2.,81.70145875985));
#6226=CARTESIAN_POINT('Origin',(0.999999999999996,0.,103.801295067582));
#6227=CARTESIAN_POINT('',(1.,-2.,139.312400150624));
#6228=CARTESIAN_POINT('',(1.,-2.,139.312400150624));
#6229=CARTESIAN_POINT('',(1.,-2.,148.317699092963));
#6230=CARTESIAN_POINT('',(0.999999999999998,-2.,109.066851612306));
#6231=CARTESIAN_POINT('',(1.,-2.,148.317699092963));
#6232=CARTESIAN_POINT('Origin',(23.2807493159906,0.,45.9176972316019));
#6233=CARTESIAN_POINT('',(-6.76818552907539,-2.,138.398809313913));
#6234=CARTESIAN_POINT('',(-6.76818552907539,-2.,138.398809313913));
#6235=CARTESIAN_POINT('',(-9.55097594168495,-2.,146.963357554211));
#6236=CARTESIAN_POINT('',(12.1159029161429,-2.,80.2795611915036));
#6237=CARTESIAN_POINT('',(-9.55097594168495,-2.,146.963357554211));
#6238=CARTESIAN_POINT('Origin',(21.3786362834003,0.,183.365153071209));
#6239=CARTESIAN_POINT('',(-8.67029856166571,-2.,90.8840409888974));
#6240=CARTESIAN_POINT('',(-8.67029856166571,-2.,90.8840409888974));
#6241=CARTESIAN_POINT('',(-11.4530889742753,-2.,82.3194927485999));
#6242=CARTESIAN_POINT('',(10.2137898835526,-2.,149.003289111307));
#6243=CARTESIAN_POINT('',(-11.4530889742753,-2.,82.3194927485999));
#6244=CARTESIAN_POINT('Origin',(-2.30323639802878,0.,104.007707435095));
#6245=CARTESIAN_POINT('',(8.6702985616657,-2.,137.780775325163));
#6246=CARTESIAN_POINT('',(8.6702985616657,-2.,137.780775325163));
#6247=CARTESIAN_POINT('',(11.4530889742753,-2.,146.345323565461));
#6248=CARTESIAN_POINT('',(-0.67608994086681,-2.,109.015549298875));
#6249=CARTESIAN_POINT('',(11.4530889742753,-2.,146.345323565461));
#6250=CARTESIAN_POINT('Origin',(-5.38101596982691,0.,105.22477344569));
#6251=CARTESIAN_POINT('',(15.4918878905933,-2.,133.953860946905));
#6252=CARTESIAN_POINT('',(15.4918878905933,-2.,133.953860946905));
#6253=CARTESIAN_POINT('',(20.7850698013853,-2.,141.239300830684));
#6254=CARTESIAN_POINT('',(-2.285999487726,-2.,109.484698175214));
#6255=CARTESIAN_POINT('',(20.7850698013853,-2.,141.239300830684));
#6256=CARTESIAN_POINT('Origin',(41.6645826936637,0.,173.380088117269));
#6257=CARTESIAN_POINT('',(-15.4918878905934,-2.,94.7109553671556));
#6258=CARTESIAN_POINT('',(-15.4918878905934,-2.,94.7109553671556));
#6259=CARTESIAN_POINT('',(-20.7850698013854,-2.,87.4255154833764));
#6260=CARTESIAN_POINT('',(20.4277828496444,-2.,144.150140763296));
#6261=CARTESIAN_POINT('',(-20.7850698013854,-2.,87.4255154833764));
#6262=CARTESIAN_POINT('Origin',(57.872109455654,0.,157.615024839444));
#6263=CARTESIAN_POINT('',(-20.7970232944598,-2.,100.458554255187));
#6264=CARTESIAN_POINT('',(-20.7970232944598,-2.,100.458554255187));
#6265=CARTESIAN_POINT('',(-28.082463178239,-2.,95.165372344395));
#6266=CARTESIAN_POINT('',(28.6421621016808,-2.,136.378224995425));
#6267=CARTESIAN_POINT('',(-28.082463178239,-2.,95.165372344395));
#6268=CARTESIAN_POINT('Origin',(-7.93206420675555,0.,107.333358198454));
#6269=CARTESIAN_POINT('',(20.7970232944598,-2.,128.206262058874));
#6270=CARTESIAN_POINT('',(20.7970232944598,-2.,128.206262058874));
#6271=CARTESIAN_POINT('',(28.082463178239,-2.,133.499443969666));
#6272=CARTESIAN_POINT('',(-3.67213947723154,-2.,110.428374680555));
#6273=CARTESIAN_POINT('',(28.082463178239,-2.,133.499443969666));
#6274=CARTESIAN_POINT('Origin',(-9.70666673318587,0.,110.127058726411));
#6275=CARTESIAN_POINT('',(24.0664011568829,-2.,121.100593686106));
#6276=CARTESIAN_POINT('',(24.0664011568829,-2.,121.100593686106));
#6277=CARTESIAN_POINT('',(32.6309493971805,-2.,123.883384098715));
#6278=CARTESIAN_POINT('',(-4.69882486940547,-2.,111.754205183573));
#6279=CARTESIAN_POINT('',(32.6309493971805,-2.,123.883384098715));
#6280=CARTESIAN_POINT('Origin',(68.4147109254286,0.,137.613157473021));
#6281=CARTESIAN_POINT('',(-24.0664011568829,-2.,107.564222627955));
#6282=CARTESIAN_POINT('',(-24.0664011568829,-2.,107.564222627955));
#6283=CARTESIAN_POINT('',(-32.6309493971805,-2.,104.781432215346));
#6284=CARTESIAN_POINT('',(34.0528469655268,-2.,126.448311073173));
#6285=CARTESIAN_POINT('',(-32.6309493971805,-2.,104.781432215346));
#6286=CARTESIAN_POINT('Origin',(72.2604038165021,0.,115.33240815703));
#6287=CARTESIAN_POINT('',(-24.9799919935936,-2.,115.33240815703));
#6288=CARTESIAN_POINT('',(-24.9799919935936,-2.,115.33240815703));
#6289=CARTESIAN_POINT('',(-33.9852909359328,-2.,115.33240815703));
#6290=CARTESIAN_POINT('',(36.1302019082511,-2.,115.33240815703));
#6291=CARTESIAN_POINT('',(-33.9852909359328,-2.,115.33240815703));
#6292=CARTESIAN_POINT('Origin',(-10.5311130894481,0.,113.33240815703));
#6293=CARTESIAN_POINT('',(24.9799919935936,-2.,113.33240815703));
#6294=CARTESIAN_POINT('',(24.9799919935936,-2.,113.33240815703));
#6295=CARTESIAN_POINT('',(33.9852909359328,-2.,113.33240815703));
#6296=CARTESIAN_POINT('',(-5.26555654472407,-2.,113.33240815703));
#6297=CARTESIAN_POINT('',(33.9852909359328,-2.,113.33240815703));
#6298=CARTESIAN_POINT('Origin',(-10.3247007219358,0.,116.635644555059));
#6299=CARTESIAN_POINT('',(23.448367168133,-2.,105.662109595365));
#6300=CARTESIAN_POINT('',(23.448367168133,-2.,105.662109595365));
#6301=CARTESIAN_POINT('',(32.0129154084306,-2.,102.879319182755));
#6302=CARTESIAN_POINT('',(-5.31685885815536,-2.,115.008498097897));
#6303=CARTESIAN_POINT('',(32.0129154084306,-2.,102.879319182755));
#6304=CARTESIAN_POINT('Origin',(69.0327449141785,0.,92.9537718736301));
#6305=CARTESIAN_POINT('',(-23.448367168133,-2.,123.002706718696));
#6306=CARTESIAN_POINT('',(-23.448367168133,-2.,123.002706718696));
#6307=CARTESIAN_POINT('',(-32.0129154084306,-2.,125.785497131306));
#6308=CARTESIAN_POINT('',(34.6708809542767,-2.,104.118618273478));
#6309=CARTESIAN_POINT('',(-32.0129154084306,-2.,125.785497131306));
#6310=CARTESIAN_POINT('Origin',(59.047679960239,0.,72.6678254633667));
#6311=CARTESIAN_POINT('',(-19.6214527898749,-2.,129.824296047624));
#6312=CARTESIAN_POINT('',(-19.6214527898749,-2.,129.824296047624));
#6313=CARTESIAN_POINT('',(-26.906892673654,-2.,135.117477958416));
#6314=CARTESIAN_POINT('',(29.8177326062657,-2.,93.9046253073861));
#6315=CARTESIAN_POINT('',(-26.906892673654,-2.,135.117477958416));
#6316=CARTESIAN_POINT('Origin',(-9.10763471134047,0.,119.713424126857));
#6317=CARTESIAN_POINT('',(19.6214527898749,-2.,98.8405202664371));
#6318=CARTESIAN_POINT('',(19.6214527898749,-2.,98.8405202664371));
#6319=CARTESIAN_POINT('',(26.9068926736541,-2.,93.5473383556451));
#6320=CARTESIAN_POINT('',(-4.84770998181646,-2.,116.618407644756));
#6321=CARTESIAN_POINT('',(26.9068926736541,-2.,93.5473383556451));
#6322=CARTESIAN_POINT('Origin',(43.2826166824136,0.,56.4602987013764));
#6323=CARTESIAN_POINT('',(-13.8738539018434,-2.,135.12943145149));
#6324=CARTESIAN_POINT('',(-13.8738539018434,-2.,135.12943145149));
#6325=CARTESIAN_POINT('',(-19.1670358126354,-2.,142.414871335269));
#6326=CARTESIAN_POINT('',(22.0458168383943,-2.,85.6902460553496));
#6327=CARTESIAN_POINT('',(-19.1670358126354,-2.,142.414871335269));
#6328=CARTESIAN_POINT('Origin',(-6.99904995857679,0.,122.264472363786));
#6329=CARTESIAN_POINT('',(13.8738539018434,-2.,93.5353848625706));
#6330=CARTESIAN_POINT('',(13.8738539018434,-2.,93.5353848625706));
#6331=CARTESIAN_POINT('',(19.1670358126354,-2.,86.2499449787914));
#6332=CARTESIAN_POINT('',(-3.90403347647587,-2.,118.004547634262));
#6333=CARTESIAN_POINT('',(19.1670358126354,-2.,86.2499449787914));
#6334=CARTESIAN_POINT('Origin',(-2.22044604925031E-15,-2.,114.33240815703));
#6335=CARTESIAN_POINT('',(-25.,2.,114.33240815703));
#6336=CARTESIAN_POINT('Origin',(-2.22044604925031E-15,2.,114.33240815703));
#6337=CARTESIAN_POINT('',(-25.,-2.,114.33240815703));
#6338=CARTESIAN_POINT('Origin',(-2.22044604925031E-15,-2.,114.33240815703));
#6339=CARTESIAN_POINT('Origin',(-2.22044604925031E-15,-2.,114.33240815703));
#6340=CARTESIAN_POINT('Origin',(-2.22044604925031E-15,-2.,114.33240815703));
#6341=CARTESIAN_POINT('Origin',(-2.22044604925031E-15,-2.,114.33240815703));
#6342=CARTESIAN_POINT('',(-1.,-2.,89.3524161634369));
#6343=CARTESIAN_POINT('Origin',(-2.22044604925031E-15,-2.,114.33240815703));
#6344=CARTESIAN_POINT('',(-1.,-0.5,89.3524161634369));
#6345=CARTESIAN_POINT('',(-1.,-2.,89.3524161634369));
#6346=CARTESIAN_POINT('',(1.,-0.5,89.3524161634369));
#6347=CARTESIAN_POINT('Origin',(-2.22044604925031E-15,-0.5,114.33240815703));
#6348=CARTESIAN_POINT('',(1.,-2.,89.3524161634369));
#6349=CARTESIAN_POINT('',(1.,-2.,89.3524161634369));
#6350=CARTESIAN_POINT('Origin',(-2.22044604925031E-15,-2.,114.33240815703));
#6351=CARTESIAN_POINT('Origin',(-2.22044604925031E-15,-2.,114.33240815703));
#6352=CARTESIAN_POINT('Origin',(-2.22044604925031E-15,-2.,114.33240815703));
#6353=CARTESIAN_POINT('Origin',(-2.22044604925031E-15,-2.,114.33240815703));
#6354=CARTESIAN_POINT('Origin',(-2.22044604925031E-15,-2.,114.33240815703));
#6355=CARTESIAN_POINT('Origin',(-2.22044604925031E-15,-2.,114.33240815703));
#6356=CARTESIAN_POINT('Origin',(-2.22044604925031E-15,-2.,114.33240815703));
#6357=CARTESIAN_POINT('Origin',(-2.22044604925031E-15,-2.,114.33240815703));
#6358=CARTESIAN_POINT('Origin',(-2.22044604925031E-15,-2.,114.33240815703));
#6359=CARTESIAN_POINT('Origin',(-2.22044604925031E-15,-2.,114.33240815703));
#6360=CARTESIAN_POINT('Origin',(-2.22044604925031E-15,-2.,114.33240815703));
#6361=CARTESIAN_POINT('Origin',(-2.22044604925031E-15,-2.,114.33240815703));
#6362=CARTESIAN_POINT('Origin',(-2.22044604925031E-15,-2.,114.33240815703));
#6363=CARTESIAN_POINT('Origin',(-2.22044604925031E-15,-2.,114.33240815703));
#6364=CARTESIAN_POINT('Origin',(-2.22044604925031E-15,-2.,114.33240815703));
#6365=CARTESIAN_POINT('Origin',(0.,-2.,114.33240815703));
#6366=CARTESIAN_POINT('',(-1.,-2.,80.3471172210976));
#6367=CARTESIAN_POINT('Origin',(-2.22044604925031E-15,-2.,114.33240815703));
#6368=CARTESIAN_POINT('',(-1.,-2.,119.597964701755));
#6369=CARTESIAN_POINT('Origin',(0.,-2.,114.33240815703));
#6370=CARTESIAN_POINT('Origin',(-2.22044604925031E-15,-2.,114.33240815703));
#6371=CARTESIAN_POINT('Origin',(0.,-2.,114.33240815703));
#6372=CARTESIAN_POINT('Origin',(-2.22044604925031E-15,-2.,114.33240815703));
#6373=CARTESIAN_POINT('Origin',(0.,-2.,114.33240815703));
#6374=CARTESIAN_POINT('Origin',(-2.22044604925031E-15,-2.,114.33240815703));
#6375=CARTESIAN_POINT('Origin',(0.,-2.,114.33240815703));
#6376=CARTESIAN_POINT('Origin',(-2.22044604925031E-15,-2.,114.33240815703));
#6377=CARTESIAN_POINT('Origin',(0.,-2.,114.33240815703));
#6378=CARTESIAN_POINT('Origin',(-2.22044604925031E-15,-2.,114.33240815703));
#6379=CARTESIAN_POINT('Origin',(0.,-2.,114.33240815703));
#6380=CARTESIAN_POINT('',(1.,-2.,80.3471172210976));
#6381=CARTESIAN_POINT('',(1.,-2.,78.2022062487794));
#6382=CARTESIAN_POINT('Origin',(-2.22044604925031E-15,-2.,114.33240815703));
#6383=CARTESIAN_POINT('Origin',(0.,-2.,114.33240815703));
#6384=CARTESIAN_POINT('Origin',(-2.22044604925031E-15,-2.,114.33240815703));
#6385=CARTESIAN_POINT('Origin',(0.,-2.,114.33240815703));
#6386=CARTESIAN_POINT('Origin',(-2.22044604925031E-15,-2.,114.33240815703));
#6387=CARTESIAN_POINT('Origin',(0.,-2.,114.33240815703));
#6388=CARTESIAN_POINT('Origin',(-2.22044604925031E-15,-2.,114.33240815703));
#6389=CARTESIAN_POINT('Origin',(0.,-2.,114.33240815703));
#6390=CARTESIAN_POINT('Origin',(-2.22044604925031E-15,-2.,114.33240815703));
#6391=CARTESIAN_POINT('Origin',(0.,-2.,114.33240815703));
#6392=CARTESIAN_POINT('Origin',(-2.22044604925031E-15,-2.,114.33240815703));
#6393=CARTESIAN_POINT('Origin',(0.,-2.,114.33240815703));
#6394=CARTESIAN_POINT('Origin',(-2.22044604925031E-15,-2.,114.33240815703));
#6395=CARTESIAN_POINT('Origin',(0.,-2.,114.33240815703));
#6396=CARTESIAN_POINT('Origin',(-2.22044604925031E-15,-2.,114.33240815703));
#6397=CARTESIAN_POINT('Origin',(0.,-2.,114.33240815703));
#6398=CARTESIAN_POINT('Origin',(-2.22044604925031E-15,-2.,114.33240815703));
#6399=CARTESIAN_POINT('Origin',(0.,-2.,114.33240815703));
#6400=CARTESIAN_POINT('Origin',(-2.22044604925031E-15,-2.,114.33240815703));
#6401=CARTESIAN_POINT('Origin',(0.,-2.,114.33240815703));
#6402=CARTESIAN_POINT('Origin',(-2.22044604925031E-15,-2.,114.33240815703));
#6403=CARTESIAN_POINT('Origin',(0.,-2.,114.33240815703));
#6404=CARTESIAN_POINT('Origin',(-2.22044604925031E-15,-2.,114.33240815703));
#6405=CARTESIAN_POINT('Origin',(0.,-2.,114.33240815703));
#6406=CARTESIAN_POINT('Origin',(-2.22044604925031E-15,-2.,114.33240815703));
#6407=CARTESIAN_POINT('Origin',(1.,0.,42.0720043405283));
#6408=CARTESIAN_POINT('',(1.,-0.5,80.3471172210976));
#6409=CARTESIAN_POINT('',(1.,-0.5,62.7698835670159));
#6410=CARTESIAN_POINT('',(1.,-2.,80.3471172210976));
#6411=CARTESIAN_POINT('Origin',(-2.08166817117217E-15,-0.5,83.4677627935035));
#6412=CARTESIAN_POINT('',(-1.,-0.5,80.3471172210976));
#6413=CARTESIAN_POINT('',(-1.,-0.5,104.165642019991));
#6414=CARTESIAN_POINT('Origin',(-2.22044604925031E-15,-0.5,114.33240815703));
#6415=CARTESIAN_POINT('Origin',(-1.,0.,124.863521246479));
#6416=CARTESIAN_POINT('',(-1.,-2.,80.3471172210976));
#6417=CARTESIAN_POINT('Origin',(-2.22044604925031E-15,-2.,114.33240815703));
#6418=CARTESIAN_POINT('',(-34.,2.,114.33240815703));
#6419=CARTESIAN_POINT('Origin',(-2.22044604925031E-15,2.,114.33240815703));
#6420=CARTESIAN_POINT('',(-34.,-2.,114.33240815703));
#6421=CARTESIAN_POINT('Origin',(-2.22044604925031E-15,-2.,114.33240815703));
#6422=CARTESIAN_POINT('Origin',(0.,2.,114.33240815703));
#6423=CARTESIAN_POINT('Origin',(0.,-2.,114.33240815703));
#6424=CARTESIAN_POINT('',(0.,0.,0.));
#6425=CARTESIAN_POINT('Origin',(0.,-3.,119.33240815703));
#6426=CARTESIAN_POINT('',(0.,-3.,119.33240815703));
#6427=CARTESIAN_POINT('',(0.,-3.,148.13240815703));
#6428=CARTESIAN_POINT('',(0.,-3.,116.83240815703));
#6429=CARTESIAN_POINT('',(0.,-2.9,119.33240815703));
#6430=CARTESIAN_POINT('',(0.,-3.,119.33240815703));
#6431=CARTESIAN_POINT('',(0.,-2.9,148.13240815703));
#6432=CARTESIAN_POINT('',(0.,-2.9,116.83240815703));
#6433=CARTESIAN_POINT('',(0.,-3.,148.13240815703));
#6434=CARTESIAN_POINT('Origin',(-23.9002092041053,-3.,138.232617361136));
#6435=CARTESIAN_POINT('',(-23.9002092041053,-3.,138.232617361136));
#6436=CARTESIAN_POINT('',(-3.53553390593273,-3.,117.867942062963));
#6437=CARTESIAN_POINT('',(-11.9501046020527,-3.,126.282512759083));
#6438=CARTESIAN_POINT('',(-23.9002092041053,-2.9,138.232617361136));
#6439=CARTESIAN_POINT('',(-23.9002092041053,-3.,138.232617361136));
#6440=CARTESIAN_POINT('',(-3.53553390593273,-2.9,117.867942062963));
#6441=CARTESIAN_POINT('',(-11.9501046020527,-2.9,126.282512759083));
#6442=CARTESIAN_POINT('',(-3.53553390593273,-3.,117.867942062963));
#6443=CARTESIAN_POINT('Origin',(0.,-3.,114.33240815703));
#6444=CARTESIAN_POINT('Origin',(0.,-3.,114.33240815703));
#6445=CARTESIAN_POINT('Origin',(0.,-3.,114.33240815703));
#6446=CARTESIAN_POINT('',(-16.5043001764605,-3.,138.196865826448));
#6447=CARTESIAN_POINT('Origin',(-15.7264827171553,-3.,138.974683285753));
#6448=CARTESIAN_POINT('',(-5.87700253253308,-3.,142.339348708895));
#6449=CARTESIAN_POINT('Origin',(-5.09918507322789,-3.,143.1171661682));
#6450=CARTESIAN_POINT('Origin',(-15.7264827171553,-3.,138.974683285753));
#6451=CARTESIAN_POINT('',(-16.5043001764605,-3.5,138.196865826448));
#6452=CARTESIAN_POINT('Origin',(-15.7264827171553,-3.5,138.974683285753));
#6453=CARTESIAN_POINT('',(-16.5043001764605,-3.,138.196865826448));
#6454=CARTESIAN_POINT('Origin',(-15.7264827171553,-3.5,138.974683285753));
#6455=CARTESIAN_POINT('Origin',(-5.09918507322789,-3.,143.1171661682));
#6456=CARTESIAN_POINT('',(-5.87700253253308,-3.5,142.339348708895));
#6457=CARTESIAN_POINT('Origin',(-5.09918507322789,-3.5,143.1171661682));
#6458=CARTESIAN_POINT('',(-5.87700253253309,-3.,142.339348708895));
#6459=CARTESIAN_POINT('Origin',(-5.09918507322789,-3.5,143.1171661682));
#6460=CARTESIAN_POINT('Origin',(0.,-3.,114.33240815703));
#6461=CARTESIAN_POINT('Origin',(0.,-2.9,114.33240815703));
#6462=CARTESIAN_POINT('Origin',(0.,-3.,114.33240815703));
#6463=CARTESIAN_POINT('Origin',(0.,-2.9,114.33240815703));
#6464=CARTESIAN_POINT('Origin',(0.,-2.9,114.33240815703));
#6465=CARTESIAN_POINT('',(0.,0.,0.));
#6466=CARTESIAN_POINT('Origin',(-3.53553390593273,-3.,117.867942062963));
#6467=CARTESIAN_POINT('',(-3.53553390593273,-3.,117.867942062963));
#6468=CARTESIAN_POINT('',(-23.9002092041053,-3.,138.232617361136));
#6469=CARTESIAN_POINT('',(-1.76776695296637,-3.,116.100175109997));
#6470=CARTESIAN_POINT('',(-3.53553390593273,-2.9,117.867942062963));
#6471=CARTESIAN_POINT('',(-3.53553390593273,-3.,117.867942062963));
#6472=CARTESIAN_POINT('',(-23.9002092041053,-2.9,138.232617361136));
#6473=CARTESIAN_POINT('',(-1.76776695296637,-2.9,116.100175109997));
#6474=CARTESIAN_POINT('',(-23.9002092041053,-3.,138.232617361136));
#6475=CARTESIAN_POINT('Origin',(-33.8,-3.,114.33240815703));
#6476=CARTESIAN_POINT('',(-33.8,-3.,114.33240815703));
#6477=CARTESIAN_POINT('',(-5.,-3.,114.33240815703));
#6478=CARTESIAN_POINT('',(-16.9,-3.,114.33240815703));
#6479=CARTESIAN_POINT('',(-33.8,-2.9,114.33240815703));
#6480=CARTESIAN_POINT('',(-33.8,-3.,114.33240815703));
#6481=CARTESIAN_POINT('',(-5.,-2.9,114.33240815703));
#6482=CARTESIAN_POINT('',(-16.9,-2.9,114.33240815703));
#6483=CARTESIAN_POINT('',(-5.,-3.,114.33240815703));
#6484=CARTESIAN_POINT('Origin',(0.,-3.,114.33240815703));
#6485=CARTESIAN_POINT('Origin',(0.,-3.,114.33240815703));
#6486=CARTESIAN_POINT('Origin',(0.,-3.,114.33240815703));
#6487=CARTESIAN_POINT('',(-28.5450224208979,-3.,119.536825430901));
#6488=CARTESIAN_POINT('Origin',(-28.5450224208979,-3.,120.636825430901));
#6489=CARTESIAN_POINT('',(-23.9595659283167,-3.,129.980637397738));
#6490=CARTESIAN_POINT('Origin',(-23.9595659283167,-3.,131.080637397738));
#6491=CARTESIAN_POINT('Origin',(-28.5450224208979,-3.,120.636825430901));
#6492=CARTESIAN_POINT('',(-28.5450224208979,-3.5,119.536825430901));
#6493=CARTESIAN_POINT('Origin',(-28.5450224208979,-3.5,120.636825430901));
#6494=CARTESIAN_POINT('',(-28.5450224208979,-3.,119.536825430901));
#6495=CARTESIAN_POINT('Origin',(-28.5450224208979,-3.5,120.636825430901));
#6496=CARTESIAN_POINT('Origin',(-23.9595659283167,-3.,131.080637397738));
#6497=CARTESIAN_POINT('',(-23.9595659283167,-3.5,129.980637397738));
#6498=CARTESIAN_POINT('Origin',(-23.9595659283167,-3.5,131.080637397738));
#6499=CARTESIAN_POINT('',(-23.9595659283167,-3.,129.980637397738));
#6500=CARTESIAN_POINT('Origin',(-23.9595659283167,-3.5,131.080637397738));
#6501=CARTESIAN_POINT('Origin',(0.,-3.,114.33240815703));
#6502=CARTESIAN_POINT('Origin',(0.,-2.9,114.33240815703));
#6503=CARTESIAN_POINT('Origin',(0.,-3.,114.33240815703));
#6504=CARTESIAN_POINT('Origin',(0.,-2.9,114.33240815703));
#6505=CARTESIAN_POINT('Origin',(0.,-2.9,114.33240815703));
#6506=CARTESIAN_POINT('',(0.,0.,0.));
#6507=CARTESIAN_POINT('Origin',(-3.53553390593274,-3.,110.796874251098));
#6508=CARTESIAN_POINT('',(-3.53553390593274,-3.,110.796874251098));
#6509=CARTESIAN_POINT('',(-23.9002092041053,-3.,90.4321989529251));
#6510=CARTESIAN_POINT('',(-1.76776695296637,-3.,112.564641204064));
#6511=CARTESIAN_POINT('',(-3.53553390593274,-2.9,110.796874251098));
#6512=CARTESIAN_POINT('',(-3.53553390593274,-3.,110.796874251098));
#6513=CARTESIAN_POINT('',(-23.9002092041053,-2.9,90.4321989529251));
#6514=CARTESIAN_POINT('',(-1.76776695296637,-2.9,112.564641204064));
#6515=CARTESIAN_POINT('',(-23.9002092041053,-3.,90.4321989529251));
#6516=CARTESIAN_POINT('Origin',(-6.35975223036837E-15,-3.,80.5324081570305));
#6517=CARTESIAN_POINT('',(-6.35975223036837E-15,-3.,80.5324081570305));
#6518=CARTESIAN_POINT('',(-2.83276944882399E-15,-3.,109.33240815703));
#6519=CARTESIAN_POINT('',(-4.29009913980934E-15,-3.,97.4324081570305));
#6520=CARTESIAN_POINT('',(-6.35975223036837E-15,-2.9,80.5324081570305));
#6521=CARTESIAN_POINT('',(-6.35975223036837E-15,-3.,80.5324081570305));
#6522=CARTESIAN_POINT('',(-2.83276944882399E-15,-2.9,109.33240815703));
#6523=CARTESIAN_POINT('',(-4.29009913980934E-15,-2.9,97.4324081570305));
#6524=CARTESIAN_POINT('',(-2.83276944882399E-15,-3.,109.33240815703));
#6525=CARTESIAN_POINT('Origin',(-4.44089209850063E-15,-3.,114.33240815703));
#6526=CARTESIAN_POINT('Origin',(-2.22044604925031E-15,-3.,114.33240815703));
#6527=CARTESIAN_POINT('Origin',(-2.22044604925031E-15,-3.,114.33240815703));
#6528=CARTESIAN_POINT('',(-5.20441727387072,-3.,85.7873857361326));
#6529=CARTESIAN_POINT('Origin',(-6.30441727387072,-3.,85.7873857361326));
#6530=CARTESIAN_POINT('',(-15.6482292407074,-3.,90.3728422287137));
#6531=CARTESIAN_POINT('Origin',(-16.7482292407074,-3.,90.3728422287137));
#6532=CARTESIAN_POINT('Origin',(-6.30441727387072,-3.,85.7873857361326));
#6533=CARTESIAN_POINT('',(-5.20441727387072,-3.5,85.7873857361326));
#6534=CARTESIAN_POINT('Origin',(-6.30441727387072,-3.5,85.7873857361326));
#6535=CARTESIAN_POINT('',(-5.20441727387072,-3.,85.7873857361326));
#6536=CARTESIAN_POINT('Origin',(-6.30441727387072,-3.5,85.7873857361326));
#6537=CARTESIAN_POINT('Origin',(-16.7482292407074,-3.,90.3728422287137));
#6538=CARTESIAN_POINT('',(-15.6482292407074,-3.5,90.3728422287137));
#6539=CARTESIAN_POINT('Origin',(-16.7482292407074,-3.5,90.3728422287137));
#6540=CARTESIAN_POINT('',(-15.6482292407074,-3.,90.3728422287137));
#6541=CARTESIAN_POINT('Origin',(-16.7482292407074,-3.5,90.3728422287137));
#6542=CARTESIAN_POINT('Origin',(-2.22044604925031E-15,-3.,114.33240815703));
#6543=CARTESIAN_POINT('Origin',(-2.22044604925031E-15,-2.9,114.33240815703));
#6544=CARTESIAN_POINT('Origin',(-2.22044604925031E-15,-3.,114.33240815703));
#6545=CARTESIAN_POINT('Origin',(-2.22044604925031E-15,-2.9,114.33240815703));
#6546=CARTESIAN_POINT('Origin',(-4.44089209850063E-15,-2.9,114.33240815703));
#6547=CARTESIAN_POINT('',(0.,0.,0.));
#6548=CARTESIAN_POINT('Origin',(0.,-3.,109.33240815703));
#6549=CARTESIAN_POINT('',(0.,-3.,109.33240815703));
#6550=CARTESIAN_POINT('',(0.,-3.,80.5324081570305));
#6551=CARTESIAN_POINT('',(0.,-3.,111.83240815703));
#6552=CARTESIAN_POINT('',(0.,-2.9,109.33240815703));
#6553=CARTESIAN_POINT('',(0.,-3.,109.33240815703));
#6554=CARTESIAN_POINT('',(0.,-2.9,80.5324081570305));
#6555=CARTESIAN_POINT('',(0.,-2.9,111.83240815703));
#6556=CARTESIAN_POINT('',(0.,-3.,80.5324081570305));
#6557=CARTESIAN_POINT('Origin',(23.9002092041053,-3.,90.4321989529251));
#6558=CARTESIAN_POINT('',(23.9002092041053,-3.,90.4321989529251));
#6559=CARTESIAN_POINT('',(3.53553390593275,-3.,110.796874251098));
#6560=CARTESIAN_POINT('',(11.9501046020527,-3.,102.382303554978));
#6561=CARTESIAN_POINT('',(23.9002092041053,-2.9,90.4321989529251));
#6562=CARTESIAN_POINT('',(23.9002092041053,-3.,90.4321989529251));
#6563=CARTESIAN_POINT('',(3.53553390593275,-2.9,110.796874251098));
#6564=CARTESIAN_POINT('',(11.9501046020527,-2.9,102.382303554978));
#6565=CARTESIAN_POINT('',(3.53553390593275,-3.,110.796874251098));
#6566=CARTESIAN_POINT('Origin',(0.,-3.,114.33240815703));
#6567=CARTESIAN_POINT('Origin',(0.,-3.,114.33240815703));
#6568=CARTESIAN_POINT('Origin',(0.,-3.,114.33240815703));
#6569=CARTESIAN_POINT('',(16.5043001764605,-3.,90.4679504876131));
#6570=CARTESIAN_POINT('Origin',(15.7264827171553,-3.,89.6901330283079));
#6571=CARTESIAN_POINT('',(5.87700253253308,-3.,86.3254676051657));
#6572=CARTESIAN_POINT('Origin',(5.09918507322787,-3.,85.5476501458605));
#6573=CARTESIAN_POINT('Origin',(15.7264827171553,-3.,89.6901330283079));
#6574=CARTESIAN_POINT('',(16.5043001764605,-3.5,90.4679504876131));
#6575=CARTESIAN_POINT('Origin',(15.7264827171553,-3.5,89.6901330283079));
#6576=CARTESIAN_POINT('',(16.5043001764605,-3.,90.4679504876131));
#6577=CARTESIAN_POINT('Origin',(15.7264827171553,-3.5,89.6901330283079));
#6578=CARTESIAN_POINT('Origin',(5.09918507322787,-3.,85.5476501458605));
#6579=CARTESIAN_POINT('',(5.87700253253308,-3.5,86.3254676051657));
#6580=CARTESIAN_POINT('Origin',(5.09918507322787,-3.5,85.5476501458605));
#6581=CARTESIAN_POINT('',(5.87700253253308,-3.,86.3254676051657));
#6582=CARTESIAN_POINT('Origin',(5.09918507322787,-3.5,85.5476501458605));
#6583=CARTESIAN_POINT('Origin',(0.,-3.,114.33240815703));
#6584=CARTESIAN_POINT('Origin',(0.,-2.9,114.33240815703));
#6585=CARTESIAN_POINT('Origin',(0.,-3.,114.33240815703));
#6586=CARTESIAN_POINT('Origin',(0.,-2.9,114.33240815703));
#6587=CARTESIAN_POINT('Origin',(0.,-2.9,114.33240815703));
#6588=CARTESIAN_POINT('',(0.,0.,0.));
#6589=CARTESIAN_POINT('Origin',(3.53553390593273,-3.,110.796874251098));
#6590=CARTESIAN_POINT('',(3.53553390593273,-3.,110.796874251098));
#6591=CARTESIAN_POINT('',(23.9002092041053,-3.,90.4321989529251));
#6592=CARTESIAN_POINT('',(1.76776695296637,-3.,112.564641204064));
#6593=CARTESIAN_POINT('',(3.53553390593273,-2.9,110.796874251098));
#6594=CARTESIAN_POINT('',(3.53553390593273,-3.,110.796874251098));
#6595=CARTESIAN_POINT('',(23.9002092041053,-2.9,90.4321989529251));
#6596=CARTESIAN_POINT('',(1.76776695296637,-2.9,112.564641204064));
#6597=CARTESIAN_POINT('',(23.9002092041053,-3.,90.4321989529251));
#6598=CARTESIAN_POINT('Origin',(33.8,-3.,114.33240815703));
#6599=CARTESIAN_POINT('',(33.8,-3.,114.33240815703));
#6600=CARTESIAN_POINT('',(5.,-3.,114.33240815703));
#6601=CARTESIAN_POINT('',(16.9,-3.,114.33240815703));
#6602=CARTESIAN_POINT('',(33.8,-2.9,114.33240815703));
#6603=CARTESIAN_POINT('',(33.8,-3.,114.33240815703));
#6604=CARTESIAN_POINT('',(5.,-2.9,114.33240815703));
#6605=CARTESIAN_POINT('',(16.9,-2.9,114.33240815703));
#6606=CARTESIAN_POINT('',(5.,-3.,114.33240815703));
#6607=CARTESIAN_POINT('Origin',(0.,-3.,114.33240815703));
#6608=CARTESIAN_POINT('Origin',(0.,-3.,114.33240815703));
#6609=CARTESIAN_POINT('Origin',(0.,-3.,114.33240815703));
#6610=CARTESIAN_POINT('',(28.5450224208979,-3.,109.12799088316));
#6611=CARTESIAN_POINT('Origin',(28.5450224208979,-3.,108.02799088316));
#6612=CARTESIAN_POINT('',(23.9595659283167,-3.,98.684178916323));
#6613=CARTESIAN_POINT('Origin',(23.9595659283167,-3.,97.584178916323));
#6614=CARTESIAN_POINT('Origin',(28.5450224208979,-3.,108.02799088316));
#6615=CARTESIAN_POINT('',(28.5450224208979,-3.5,109.12799088316));
#6616=CARTESIAN_POINT('Origin',(28.5450224208979,-3.5,108.02799088316));
#6617=CARTESIAN_POINT('',(28.5450224208979,-3.,109.12799088316));
#6618=CARTESIAN_POINT('Origin',(28.5450224208979,-3.5,108.02799088316));
#6619=CARTESIAN_POINT('Origin',(23.9595659283167,-3.,97.584178916323));
#6620=CARTESIAN_POINT('',(23.9595659283167,-3.5,98.684178916323));
#6621=CARTESIAN_POINT('Origin',(23.9595659283167,-3.5,97.584178916323));
#6622=CARTESIAN_POINT('',(23.9595659283167,-3.,98.684178916323));
#6623=CARTESIAN_POINT('Origin',(23.9595659283167,-3.5,97.584178916323));
#6624=CARTESIAN_POINT('Origin',(0.,-3.,114.33240815703));
#6625=CARTESIAN_POINT('Origin',(0.,-2.9,114.33240815703));
#6626=CARTESIAN_POINT('Origin',(0.,-3.,114.33240815703));
#6627=CARTESIAN_POINT('Origin',(0.,-2.9,114.33240815703));
#6628=CARTESIAN_POINT('Origin',(0.,-2.9,114.33240815703));
#6629=CARTESIAN_POINT('',(0.,0.,0.));
#6630=CARTESIAN_POINT('Origin',(4.99999999999998,-3.,114.33240815703));
#6631=CARTESIAN_POINT('',(4.99999999999998,-3.,114.33240815703));
#6632=CARTESIAN_POINT('',(33.8,-3.,114.33240815703));
#6633=CARTESIAN_POINT('',(2.5,-3.,114.33240815703));
#6634=CARTESIAN_POINT('',(4.99999999999998,-2.9,114.33240815703));
#6635=CARTESIAN_POINT('',(4.99999999999998,-3.,114.33240815703));
#6636=CARTESIAN_POINT('',(33.8,-2.9,114.33240815703));
#6637=CARTESIAN_POINT('',(2.5,-2.9,114.33240815703));
#6638=CARTESIAN_POINT('',(33.8,-3.,114.33240815703));
#6639=CARTESIAN_POINT('Origin',(23.9002092041053,-3.,138.232617361136));
#6640=CARTESIAN_POINT('',(23.9002092041053,-3.,138.232617361136));
#6641=CARTESIAN_POINT('',(3.53553390593273,-3.,117.867942062963));
#6642=CARTESIAN_POINT('',(11.9501046020526,-3.,126.282512759083));
#6643=CARTESIAN_POINT('',(23.9002092041053,-2.9,138.232617361136));
#6644=CARTESIAN_POINT('',(23.9002092041053,-3.,138.232617361136));
#6645=CARTESIAN_POINT('',(3.53553390593273,-2.9,117.867942062963));
#6646=CARTESIAN_POINT('',(11.9501046020526,-2.9,126.282512759083));
#6647=CARTESIAN_POINT('',(3.53553390593273,-3.,117.867942062963));
#6648=CARTESIAN_POINT('Origin',(0.,-3.,114.33240815703));
#6649=CARTESIAN_POINT('Origin',(0.,-3.,114.33240815703));
#6650=CARTESIAN_POINT('Origin',(0.,-3.,114.33240815703));
#6651=CARTESIAN_POINT('',(23.8644576694173,-3.,130.836708333491));
#6652=CARTESIAN_POINT('Origin',(24.6422751287225,-3.,130.058890874186));
#6653=CARTESIAN_POINT('',(28.0069405518647,-3.,120.209410689563));
#6654=CARTESIAN_POINT('Origin',(28.7847580111699,-3.,119.431593230258));
#6655=CARTESIAN_POINT('Origin',(24.6422751287225,-3.,130.058890874186));
#6656=CARTESIAN_POINT('',(23.8644576694173,-3.5,130.836708333491));
#6657=CARTESIAN_POINT('Origin',(24.6422751287225,-3.5,130.058890874186));
#6658=CARTESIAN_POINT('',(23.8644576694173,-3.,130.836708333491));
#6659=CARTESIAN_POINT('Origin',(24.6422751287225,-3.5,130.058890874186));
#6660=CARTESIAN_POINT('Origin',(28.7847580111699,-3.,119.431593230258));
#6661=CARTESIAN_POINT('',(28.0069405518647,-3.5,120.209410689563));
#6662=CARTESIAN_POINT('Origin',(28.7847580111699,-3.5,119.431593230258));
#6663=CARTESIAN_POINT('',(28.0069405518647,-3.,120.209410689563));
#6664=CARTESIAN_POINT('Origin',(28.7847580111699,-3.5,119.431593230258));
#6665=CARTESIAN_POINT('Origin',(0.,-3.,114.33240815703));
#6666=CARTESIAN_POINT('Origin',(0.,-2.9,114.33240815703));
#6667=CARTESIAN_POINT('Origin',(0.,-3.,114.33240815703));
#6668=CARTESIAN_POINT('Origin',(0.,-2.9,114.33240815703));
#6669=CARTESIAN_POINT('Origin',(0.,-2.9,114.33240815703));
#6670=CARTESIAN_POINT('',(0.,0.,0.));
#6671=CARTESIAN_POINT('Origin',(-5.,-3.,114.33240815703));
#6672=CARTESIAN_POINT('',(-5.,-3.,114.33240815703));
#6673=CARTESIAN_POINT('',(-33.8,-3.,114.33240815703));
#6674=CARTESIAN_POINT('',(-2.5,-3.,114.33240815703));
#6675=CARTESIAN_POINT('',(-5.,-2.9,114.33240815703));
#6676=CARTESIAN_POINT('',(-5.,-3.,114.33240815703));
#6677=CARTESIAN_POINT('',(-33.8,-2.9,114.33240815703));
#6678=CARTESIAN_POINT('',(-2.5,-2.9,114.33240815703));
#6679=CARTESIAN_POINT('',(-33.8,-3.,114.33240815703));
#6680=CARTESIAN_POINT('Origin',(-23.9002092041053,-3.,90.4321989529251));
#6681=CARTESIAN_POINT('',(-23.9002092041053,-3.,90.4321989529251));
#6682=CARTESIAN_POINT('',(-3.53553390593273,-3.,110.796874251098));
#6683=CARTESIAN_POINT('',(-11.9501046020527,-3.,102.382303554978));
#6684=CARTESIAN_POINT('',(-23.9002092041053,-2.9,90.4321989529251));
#6685=CARTESIAN_POINT('',(-23.9002092041053,-3.,90.4321989529251));
#6686=CARTESIAN_POINT('',(-3.53553390593273,-2.9,110.796874251098));
#6687=CARTESIAN_POINT('',(-11.9501046020527,-2.9,102.382303554978));
#6688=CARTESIAN_POINT('',(-3.53553390593273,-3.,110.796874251098));
#6689=CARTESIAN_POINT('Origin',(0.,-3.,114.33240815703));
#6690=CARTESIAN_POINT('Origin',(0.,-3.,114.33240815703));
#6691=CARTESIAN_POINT('Origin',(0.,-3.,114.33240815703));
#6692=CARTESIAN_POINT('',(-23.8644576694173,-3.,97.8281079805699));
#6693=CARTESIAN_POINT('Origin',(-24.6422751287225,-3.,98.6059254398751));
#6694=CARTESIAN_POINT('',(-28.0069405518647,-3.,108.455405624497));
#6695=CARTESIAN_POINT('Origin',(-28.7847580111699,-3.,109.233223083803));
#6696=CARTESIAN_POINT('Origin',(-24.6422751287225,-3.,98.6059254398751));
#6697=CARTESIAN_POINT('',(-23.8644576694173,-3.5,97.8281079805699));
#6698=CARTESIAN_POINT('Origin',(-24.6422751287225,-3.5,98.6059254398751));
#6699=CARTESIAN_POINT('',(-23.8644576694173,-3.,97.8281079805699));
#6700=CARTESIAN_POINT('Origin',(-24.6422751287225,-3.5,98.6059254398751));
#6701=CARTESIAN_POINT('Origin',(-28.7847580111699,-3.,109.233223083803));
#6702=CARTESIAN_POINT('',(-28.0069405518647,-3.5,108.455405624497));
#6703=CARTESIAN_POINT('Origin',(-28.7847580111699,-3.5,109.233223083803));
#6704=CARTESIAN_POINT('',(-28.0069405518647,-3.,108.455405624497));
#6705=CARTESIAN_POINT('Origin',(-28.7847580111699,-3.5,109.233223083803));
#6706=CARTESIAN_POINT('Origin',(0.,-3.,114.33240815703));
#6707=CARTESIAN_POINT('Origin',(0.,-2.9,114.33240815703));
#6708=CARTESIAN_POINT('Origin',(0.,-3.,114.33240815703));
#6709=CARTESIAN_POINT('Origin',(0.,-2.9,114.33240815703));
#6710=CARTESIAN_POINT('Origin',(0.,-2.9,114.33240815703));
#6711=CARTESIAN_POINT('',(0.,0.,0.));
#6712=CARTESIAN_POINT('',(0.,0.,0.));
#6713=CARTESIAN_POINT('',(0.,0.,0.));
#6714=CARTESIAN_POINT('',(0.,0.,0.));
#6715=CARTESIAN_POINT('',(0.,0.,0.));
#6716=CARTESIAN_POINT('',(0.,0.,0.));
#6717=CARTESIAN_POINT('',(0.,0.,0.));
#6718=CARTESIAN_POINT('',(0.,0.,0.));
#6719=CARTESIAN_POINT('',(0.,0.,0.));
#6720=CARTESIAN_POINT('',(0.,0.,0.));
#6721=CARTESIAN_POINT('',(0.,0.,0.));
#6722=CARTESIAN_POINT('',(0.,0.,0.));
#6723=CARTESIAN_POINT('',(0.,0.,0.));
#6724=UNCERTAINTY_MEASURE_WITH_UNIT(LENGTH_MEASURE(0.01),#6754,
'DISTANCE_ACCURACY_VALUE',
'Maximum model space distance between geometric entities at asserted c
onnectivities');
#6725=UNCERTAINTY_MEASURE_WITH_UNIT(LENGTH_MEASURE(0.01),#6754,
'DISTANCE_ACCURACY_VALUE',
'Maximum model space distance between geometric entities at asserted c
onnectivities');
#6726=UNCERTAINTY_MEASURE_WITH_UNIT(LENGTH_MEASURE(0.01),#6754,
'DISTANCE_ACCURACY_VALUE',
'Maximum model space distance between geometric entities at asserted c
onnectivities');
#6727=UNCERTAINTY_MEASURE_WITH_UNIT(LENGTH_MEASURE(0.01),#6754,
'DISTANCE_ACCURACY_VALUE',
'Maximum model space distance between geometric entities at asserted c
onnectivities');
#6728=UNCERTAINTY_MEASURE_WITH_UNIT(LENGTH_MEASURE(0.01),#6754,
'DISTANCE_ACCURACY_VALUE',
'Maximum model space distance between geometric entities at asserted c
onnectivities');
#6729=UNCERTAINTY_MEASURE_WITH_UNIT(LENGTH_MEASURE(0.01),#6754,
'DISTANCE_ACCURACY_VALUE',
'Maximum model space distance between geometric entities at asserted c
onnectivities');
#6730=UNCERTAINTY_MEASURE_WITH_UNIT(LENGTH_MEASURE(0.01),#6754,
'DISTANCE_ACCURACY_VALUE',
'Maximum model space distance between geometric entities at asserted c
onnectivities');
#6731=UNCERTAINTY_MEASURE_WITH_UNIT(LENGTH_MEASURE(0.01),#6754,
'DISTANCE_ACCURACY_VALUE',
'Maximum model space distance between geometric entities at asserted c
onnectivities');
#6732=UNCERTAINTY_MEASURE_WITH_UNIT(LENGTH_MEASURE(0.01),#6754,
'DISTANCE_ACCURACY_VALUE',
'Maximum model space distance between geometric entities at asserted c
onnectivities');
#6733=UNCERTAINTY_MEASURE_WITH_UNIT(LENGTH_MEASURE(0.01),#6754,
'DISTANCE_ACCURACY_VALUE',
'Maximum model space distance between geometric entities at asserted c
onnectivities');
#6734=UNCERTAINTY_MEASURE_WITH_UNIT(LENGTH_MEASURE(0.01),#6754,
'DISTANCE_ACCURACY_VALUE',
'Maximum model space distance between geometric entities at asserted c
onnectivities');
#6735=UNCERTAINTY_MEASURE_WITH_UNIT(LENGTH_MEASURE(0.01),#6754,
'DISTANCE_ACCURACY_VALUE',
'Maximum model space distance between geometric entities at asserted c
onnectivities');
#6736=UNCERTAINTY_MEASURE_WITH_UNIT(LENGTH_MEASURE(0.01),#6754,
'DISTANCE_ACCURACY_VALUE',
'Maximum model space distance between geometric entities at asserted c
onnectivities');
#6737=UNCERTAINTY_MEASURE_WITH_UNIT(LENGTH_MEASURE(0.01),#6754,
'DISTANCE_ACCURACY_VALUE',
'Maximum model space distance between geometric entities at asserted c
onnectivities');
#6738=UNCERTAINTY_MEASURE_WITH_UNIT(LENGTH_MEASURE(0.01),#6754,
'DISTANCE_ACCURACY_VALUE',
'Maximum model space distance between geometric entities at asserted c
onnectivities');
#6739=(
GEOMETRIC_REPRESENTATION_CONTEXT(3)
GLOBAL_UNCERTAINTY_ASSIGNED_CONTEXT((#6724))
GLOBAL_UNIT_ASSIGNED_CONTEXT((#6754,#6756,#6757))
REPRESENTATION_CONTEXT('','3D')
);
#6740=(
GEOMETRIC_REPRESENTATION_CONTEXT(3)
GLOBAL_UNCERTAINTY_ASSIGNED_CONTEXT((#6725))
GLOBAL_UNIT_ASSIGNED_CONTEXT((#6754,#6756,#6757))
REPRESENTATION_CONTEXT('','3D')
);
#6741=(
GEOMETRIC_REPRESENTATION_CONTEXT(3)
GLOBAL_UNCERTAINTY_ASSIGNED_CONTEXT((#6726))
GLOBAL_UNIT_ASSIGNED_CONTEXT((#6754,#6756,#6757))
REPRESENTATION_CONTEXT('','3D')
);
#6742=(
GEOMETRIC_REPRESENTATION_CONTEXT(3)
GLOBAL_UNCERTAINTY_ASSIGNED_CONTEXT((#6727))
GLOBAL_UNIT_ASSIGNED_CONTEXT((#6754,#6756,#6757))
REPRESENTATION_CONTEXT('','3D')
);
#6743=(
GEOMETRIC_REPRESENTATION_CONTEXT(3)
GLOBAL_UNCERTAINTY_ASSIGNED_CONTEXT((#6728))
GLOBAL_UNIT_ASSIGNED_CONTEXT((#6754,#6756,#6757))
REPRESENTATION_CONTEXT('','3D')
);
#6744=(
GEOMETRIC_REPRESENTATION_CONTEXT(3)
GLOBAL_UNCERTAINTY_ASSIGNED_CONTEXT((#6729))
GLOBAL_UNIT_ASSIGNED_CONTEXT((#6754,#6756,#6757))
REPRESENTATION_CONTEXT('','3D')
);
#6745=(
GEOMETRIC_REPRESENTATION_CONTEXT(3)
GLOBAL_UNCERTAINTY_ASSIGNED_CONTEXT((#6730))
GLOBAL_UNIT_ASSIGNED_CONTEXT((#6754,#6756,#6757))
REPRESENTATION_CONTEXT('','3D')
);
#6746=(
GEOMETRIC_REPRESENTATION_CONTEXT(3)
GLOBAL_UNCERTAINTY_ASSIGNED_CONTEXT((#6731))
GLOBAL_UNIT_ASSIGNED_CONTEXT((#6754,#6756,#6757))
REPRESENTATION_CONTEXT('','3D')
);
#6747=(
GEOMETRIC_REPRESENTATION_CONTEXT(3)
GLOBAL_UNCERTAINTY_ASSIGNED_CONTEXT((#6732))
GLOBAL_UNIT_ASSIGNED_CONTEXT((#6754,#6756,#6757))
REPRESENTATION_CONTEXT('','3D')
);
#6748=(
GEOMETRIC_REPRESENTATION_CONTEXT(3)
GLOBAL_UNCERTAINTY_ASSIGNED_CONTEXT((#6733))
GLOBAL_UNIT_ASSIGNED_CONTEXT((#6754,#6756,#6757))
REPRESENTATION_CONTEXT('','3D')
);
#6749=(
GEOMETRIC_REPRESENTATION_CONTEXT(3)
GLOBAL_UNCERTAINTY_ASSIGNED_CONTEXT((#6734))
GLOBAL_UNIT_ASSIGNED_CONTEXT((#6754,#6756,#6757))
REPRESENTATION_CONTEXT('','3D')
);
#6750=(
GEOMETRIC_REPRESENTATION_CONTEXT(3)
GLOBAL_UNCERTAINTY_ASSIGNED_CONTEXT((#6735))
GLOBAL_UNIT_ASSIGNED_CONTEXT((#6754,#6756,#6757))
REPRESENTATION_CONTEXT('','3D')
);
#6751=(
GEOMETRIC_REPRESENTATION_CONTEXT(3)
GLOBAL_UNCERTAINTY_ASSIGNED_CONTEXT((#6736))
GLOBAL_UNIT_ASSIGNED_CONTEXT((#6754,#6756,#6757))
REPRESENTATION_CONTEXT('','3D')
);
#6752=(
GEOMETRIC_REPRESENTATION_CONTEXT(3)
GLOBAL_UNCERTAINTY_ASSIGNED_CONTEXT((#6737))
GLOBAL_UNIT_ASSIGNED_CONTEXT((#6754,#6756,#6757))
REPRESENTATION_CONTEXT('','3D')
);
#6753=(
GEOMETRIC_REPRESENTATION_CONTEXT(3)
GLOBAL_UNCERTAINTY_ASSIGNED_CONTEXT((#6738))
GLOBAL_UNIT_ASSIGNED_CONTEXT((#6754,#6756,#6757))
REPRESENTATION_CONTEXT('','3D')
);
#6754=(
LENGTH_UNIT()
NAMED_UNIT(*)
SI_UNIT(.MILLI.,.METRE.)
);
#6755=(
LENGTH_UNIT()
NAMED_UNIT(*)
SI_UNIT($,.METRE.)
);
#6756=(
NAMED_UNIT(*)
PLANE_ANGLE_UNIT()
SI_UNIT($,.RADIAN.)
);
#6757=(
NAMED_UNIT(*)
SI_UNIT($,.STERADIAN.)
SOLID_ANGLE_UNIT()
);
#6758=SHAPE_DEFINITION_REPRESENTATION(#6772,#6799);
#6759=SHAPE_DEFINITION_REPRESENTATION(#6773,#6800);
#6760=SHAPE_DEFINITION_REPRESENTATION(#6774,#6801);
#6761=SHAPE_DEFINITION_REPRESENTATION(#6775,#6802);
#6762=SHAPE_DEFINITION_REPRESENTATION(#6776,#6803);
#6763=SHAPE_DEFINITION_REPRESENTATION(#6777,#6804);
#6764=SHAPE_DEFINITION_REPRESENTATION(#6778,#6805);
#6765=SHAPE_DEFINITION_REPRESENTATION(#6779,#6806);
#6766=SHAPE_DEFINITION_REPRESENTATION(#6780,#6807);
#6767=SHAPE_DEFINITION_REPRESENTATION(#6781,#6808);
#6768=SHAPE_DEFINITION_REPRESENTATION(#6782,#6809);
#6769=SHAPE_DEFINITION_REPRESENTATION(#6783,#6810);
#6770=SHAPE_DEFINITION_REPRESENTATION(#6784,#6811);
#6771=SHAPE_DEFINITION_REPRESENTATION(#6785,#6812);
#6772=PRODUCT_DEFINITION_SHAPE('',$,#6814);
#6773=PRODUCT_DEFINITION_SHAPE('',$,#6815);
#6774=PRODUCT_DEFINITION_SHAPE('',$,#6816);
#6775=PRODUCT_DEFINITION_SHAPE('',$,#6817);
#6776=PRODUCT_DEFINITION_SHAPE('',$,#6818);
#6777=PRODUCT_DEFINITION_SHAPE('',$,#6819);
#6778=PRODUCT_DEFINITION_SHAPE('',$,#6820);
#6779=PRODUCT_DEFINITION_SHAPE('',$,#6821);
#6780=PRODUCT_DEFINITION_SHAPE('',$,#6822);
#6781=PRODUCT_DEFINITION_SHAPE('',$,#6823);
#6782=PRODUCT_DEFINITION_SHAPE('',$,#6824);
#6783=PRODUCT_DEFINITION_SHAPE('',$,#6825);
#6784=PRODUCT_DEFINITION_SHAPE('',$,#6826);
#6785=PRODUCT_DEFINITION_SHAPE('',$,#6827);
#6786=PRODUCT_DEFINITION_SHAPE($,$,#50);
#6787=PRODUCT_DEFINITION_SHAPE($,$,#51);
#6788=PRODUCT_DEFINITION_SHAPE($,$,#52);
#6789=PRODUCT_DEFINITION_SHAPE($,$,#53);
#6790=PRODUCT_DEFINITION_SHAPE($,$,#54);
#6791=PRODUCT_DEFINITION_SHAPE($,$,#55);
#6792=PRODUCT_DEFINITION_SHAPE($,$,#56);
#6793=PRODUCT_DEFINITION_SHAPE($,$,#57);
#6794=PRODUCT_DEFINITION_SHAPE($,$,#58);
#6795=PRODUCT_DEFINITION_SHAPE($,$,#59);
#6796=PRODUCT_DEFINITION_SHAPE($,$,#60);
#6797=PRODUCT_DEFINITION_SHAPE($,$,#61);
#6798=PRODUCT_DEFINITION_SHAPE($,$,#62);
#6799=SHAPE_REPRESENTATION('',(#3909,#4352,#4353,#4354,#4355,#4356,#4357,
#4358,#4359,#4360,#4361,#4362,#4363,#4364),#6739);
#6800=SHAPE_REPRESENTATION('',(#3910),#6740);
#6801=SHAPE_REPRESENTATION('',(#3930),#6741);
#6802=SHAPE_REPRESENTATION('',(#3941),#6742);
#6803=SHAPE_REPRESENTATION('',(#3960),#6743);
#6804=SHAPE_REPRESENTATION('',(#4028),#6744);
#6805=SHAPE_REPRESENTATION('',(#4048),#6745);
#6806=SHAPE_REPRESENTATION('',(#4219),#6746);
#6807=SHAPE_REPRESENTATION('',(#4238),#6747);
#6808=SHAPE_REPRESENTATION('',(#4257),#6748);
#6809=SHAPE_REPRESENTATION('',(#4276),#6749);
#6810=SHAPE_REPRESENTATION('',(#4295),#6750);
#6811=SHAPE_REPRESENTATION('',(#4314),#6751);
#6812=SHAPE_REPRESENTATION('',(#4333),#6752);
#6813=PRODUCT_DEFINITION_CONTEXT('part definition',#6857,'design');
#6814=PRODUCT_DEFINITION('MAS-284','MAS-284',#6828,#6813);
#6815=PRODUCT_DEFINITION('Main_Housing','Main_Housing',#6829,#6813);
#6816=PRODUCT_DEFINITION('Pin','Pin',#6830,#6813);
#6817=PRODUCT_DEFINITION('Blade_01','Blade_01',#6831,#6813);
#6818=PRODUCT_DEFINITION('Front_Plate','Front_Plate',#6832,#6813);
#6819=PRODUCT_DEFINITION('Shaft','Shaft',#6833,#6813);
#6820=PRODUCT_DEFINITION('Disc','Disc',#6834,#6813);
#6821=PRODUCT_DEFINITION('Blade_02','Blade_02',#6835,#6813);
#6822=PRODUCT_DEFINITION('Blade_03','Blade_03',#6836,#6813);
#6823=PRODUCT_DEFINITION('Blade_05','Blade_05',#6837,#6813);
#6824=PRODUCT_DEFINITION('Blade_06','Blade_06',#6838,#6813);
#6825=PRODUCT_DEFINITION('Blade_07','Blade_07',#6839,#6813);
#6826=PRODUCT_DEFINITION('Blade_08','Blade_08',#6840,#6813);
#6827=PRODUCT_DEFINITION('Blade_04','Blade_04',#6841,#6813);
#6828=PRODUCT_DEFINITION_FORMATION('',$,#6859);
#6829=PRODUCT_DEFINITION_FORMATION('',$,#6860);
#6830=PRODUCT_DEFINITION_FORMATION('',$,#6861);
#6831=PRODUCT_DEFINITION_FORMATION('',$,#6862);
#6832=PRODUCT_DEFINITION_FORMATION('',$,#6863);
#6833=PRODUCT_DEFINITION_FORMATION('',$,#6864);
#6834=PRODUCT_DEFINITION_FORMATION('',$,#6865);
#6835=PRODUCT_DEFINITION_FORMATION('',$,#6866);
#6836=PRODUCT_DEFINITION_FORMATION('',$,#6867);
#6837=PRODUCT_DEFINITION_FORMATION('',$,#6868);
#6838=PRODUCT_DEFINITION_FORMATION('',$,#6869);
#6839=PRODUCT_DEFINITION_FORMATION('',$,#6870);
#6840=PRODUCT_DEFINITION_FORMATION('',$,#6871);
#6841=PRODUCT_DEFINITION_FORMATION('',$,#6872);
#6842=PRODUCT_RELATED_PRODUCT_CATEGORY('MAS-284','MAS-284',(#6859));
#6843=PRODUCT_RELATED_PRODUCT_CATEGORY('Main_Housing','Main_Housing',(#6860));
#6844=PRODUCT_RELATED_PRODUCT_CATEGORY('Pin','Pin',(#6861));
#6845=PRODUCT_RELATED_PRODUCT_CATEGORY('Blade_01','Blade_01',(#6862));
#6846=PRODUCT_RELATED_PRODUCT_CATEGORY('Front_Plate','Front_Plate',(#6863));
#6847=PRODUCT_RELATED_PRODUCT_CATEGORY('Shaft','Shaft',(#6864));
#6848=PRODUCT_RELATED_PRODUCT_CATEGORY('Disc','Disc',(#6865));
#6849=PRODUCT_RELATED_PRODUCT_CATEGORY('Blade_02','Blade_02',(#6866));
#6850=PRODUCT_RELATED_PRODUCT_CATEGORY('Blade_03','Blade_03',(#6867));
#6851=PRODUCT_RELATED_PRODUCT_CATEGORY('Blade_05','Blade_05',(#6868));
#6852=PRODUCT_RELATED_PRODUCT_CATEGORY('Blade_06','Blade_06',(#6869));
#6853=PRODUCT_RELATED_PRODUCT_CATEGORY('Blade_07','Blade_07',(#6870));
#6854=PRODUCT_RELATED_PRODUCT_CATEGORY('Blade_08','Blade_08',(#6871));
#6855=PRODUCT_RELATED_PRODUCT_CATEGORY('Blade_04','Blade_04',(#6872));
#6856=APPLICATION_PROTOCOL_DEFINITION('international standard',
'automotive_design',2009,#6857);
#6857=APPLICATION_CONTEXT(
'Core Data for Automotive Mechanical Design Process');
#6858=PRODUCT_CONTEXT('part definition',#6857,'mechanical');
#6859=PRODUCT('MAS-284','MAS-284',$,(#6858));
#6860=PRODUCT('Main_Housing','Main_Housing',$,(#6858));
#6861=PRODUCT('Pin','Pin',$,(#6858));
#6862=PRODUCT('Blade_01','Blade_01',$,(#6858));
#6863=PRODUCT('Front_Plate','Front_Plate',$,(#6858));
#6864=PRODUCT('Shaft','Shaft',$,(#6858));
#6865=PRODUCT('Disc','Disc',$,(#6858));
#6866=PRODUCT('Blade_02','Blade_02',$,(#6858));
#6867=PRODUCT('Blade_03','Blade_03',$,(#6858));
#6868=PRODUCT('Blade_05','Blade_05',$,(#6858));
#6869=PRODUCT('Blade_06','Blade_06',$,(#6858));
#6870=PRODUCT('Blade_07','Blade_07',$,(#6858));
#6871=PRODUCT('Blade_08','Blade_08',$,(#6858));
#6872=PRODUCT('Blade_04','Blade_04',$,(#6858));
#6873=PRESENTATION_STYLE_ASSIGNMENT((#6876));
#6874=PRESENTATION_STYLE_ASSIGNMENT((#6877));
#6875=PRESENTATION_STYLE_ASSIGNMENT((#6878));
#6876=SURFACE_STYLE_USAGE(.BOTH.,#6879);
#6877=SURFACE_STYLE_USAGE(.BOTH.,#6880);
#6878=SURFACE_STYLE_USAGE(.BOTH.,#6881);
#6879=SURFACE_SIDE_STYLE('',(#6882));
#6880=SURFACE_SIDE_STYLE('',(#6883));
#6881=SURFACE_SIDE_STYLE('',(#6884));
#6882=SURFACE_STYLE_FILL_AREA(#6885);
#6883=SURFACE_STYLE_FILL_AREA(#6886);
#6884=SURFACE_STYLE_FILL_AREA(#6887);
#6885=FILL_AREA_STYLE('Steel - Satin',(#6888));
#6886=FILL_AREA_STYLE('Opaque(65,65,65)',(#6889));
#6887=FILL_AREA_STYLE('Opaque(192,192,192)',(#6890));
#6888=FILL_AREA_STYLE_COLOUR('Steel - Satin',#6891);
#6889=FILL_AREA_STYLE_COLOUR('Opaque(65,65,65)',#6892);
#6890=FILL_AREA_STYLE_COLOUR('Opaque(192,192,192)',#6893);
#6891=COLOUR_RGB('Steel - Satin',0.627450980392157,0.627450980392157,0.627450980392157);
#6892=COLOUR_RGB('Opaque(65,65,65)',0.254901960784314,0.254901960784314,
0.254901960784314);
#6893=COLOUR_RGB('Opaque(192,192,192)',0.752941176470588,0.752941176470588,
0.752941176470588);
#6894=COLOUR_RGB('Dark Blue',0.08,0.2,0.34);
#6895=FILL_AREA_STYLE_COLOUR('',#6894);
#6896=FILL_AREA_STYLE('',(#6895));
#6897=SURFACE_STYLE_FILL_AREA(#6896);
#6898=SURFACE_SIDE_STYLE('',(#6897));
#6899=SURFACE_STYLE_USAGE(.BOTH.,#6898);
#6900=PRESENTATION_STYLE_ASSIGNMENT((#6899));
#6901=COLOUR_RGB('Light Blue',0.38,0.62,0.78);
#6902=FILL_AREA_STYLE_COLOUR('',#6901);
#6903=FILL_AREA_STYLE('',(#6902));
#6904=SURFACE_STYLE_FILL_AREA(#6903);
#6905=SURFACE_SIDE_STYLE('',(#6904));
#6906=SURFACE_STYLE_USAGE(.BOTH.,#6905);
#6907=PRESENTATION_STYLE_ASSIGNMENT((#6906));
#6908=COLOUR_RGB('Sky Blue',0.24,0.69,0.87);
#6909=FILL_AREA_STYLE_COLOUR('',#6908);
#6910=FILL_AREA_STYLE('',(#6909));
#6911=SURFACE_STYLE_FILL_AREA(#6910);
#6912=SURFACE_SIDE_STYLE('',(#6911));
#6913=SURFACE_STYLE_USAGE(.BOTH.,#6912);
#6914=PRESENTATION_STYLE_ASSIGNMENT((#6913));
#6915=COLOUR_RGB('Grey',0.48,0.52,0.57);
#6916=FILL_AREA_STYLE_COLOUR('',#6915);
#6917=FILL_AREA_STYLE('',(#6916));
#6918=SURFACE_STYLE_FILL_AREA(#6917);
#6919=SURFACE_SIDE_STYLE('',(#6918));
#6920=SURFACE_STYLE_USAGE(.BOTH.,#6919);
#6921=PRESENTATION_STYLE_ASSIGNMENT((#6920));
#6922=COLOUR_RGB('Black',0.12,0.14,0.17);
#6923=FILL_AREA_STYLE_COLOUR('',#6922);
#6924=FILL_AREA_STYLE('',(#6923));
#6925=SURFACE_STYLE_FILL_AREA(#6924);
#6926=SURFACE_SIDE_STYLE('',(#6925));
#6927=SURFACE_STYLE_USAGE(.BOTH.,#6926);
#6928=PRESENTATION_STYLE_ASSIGNMENT((#6927));
#6929=COLOUR_RGB('Off White',0.89,0.88,0.83);
#6930=FILL_AREA_STYLE_COLOUR('',#6929);
#6931=FILL_AREA_STYLE('',(#6930));
#6932=SURFACE_STYLE_FILL_AREA(#6931);
#6933=SURFACE_SIDE_STYLE('',(#6932));
#6934=SURFACE_STYLE_USAGE(.BOTH.,#6933);
#6935=PRESENTATION_STYLE_ASSIGNMENT((#6934));
ENDSEC;
END-ISO-10303-21;
